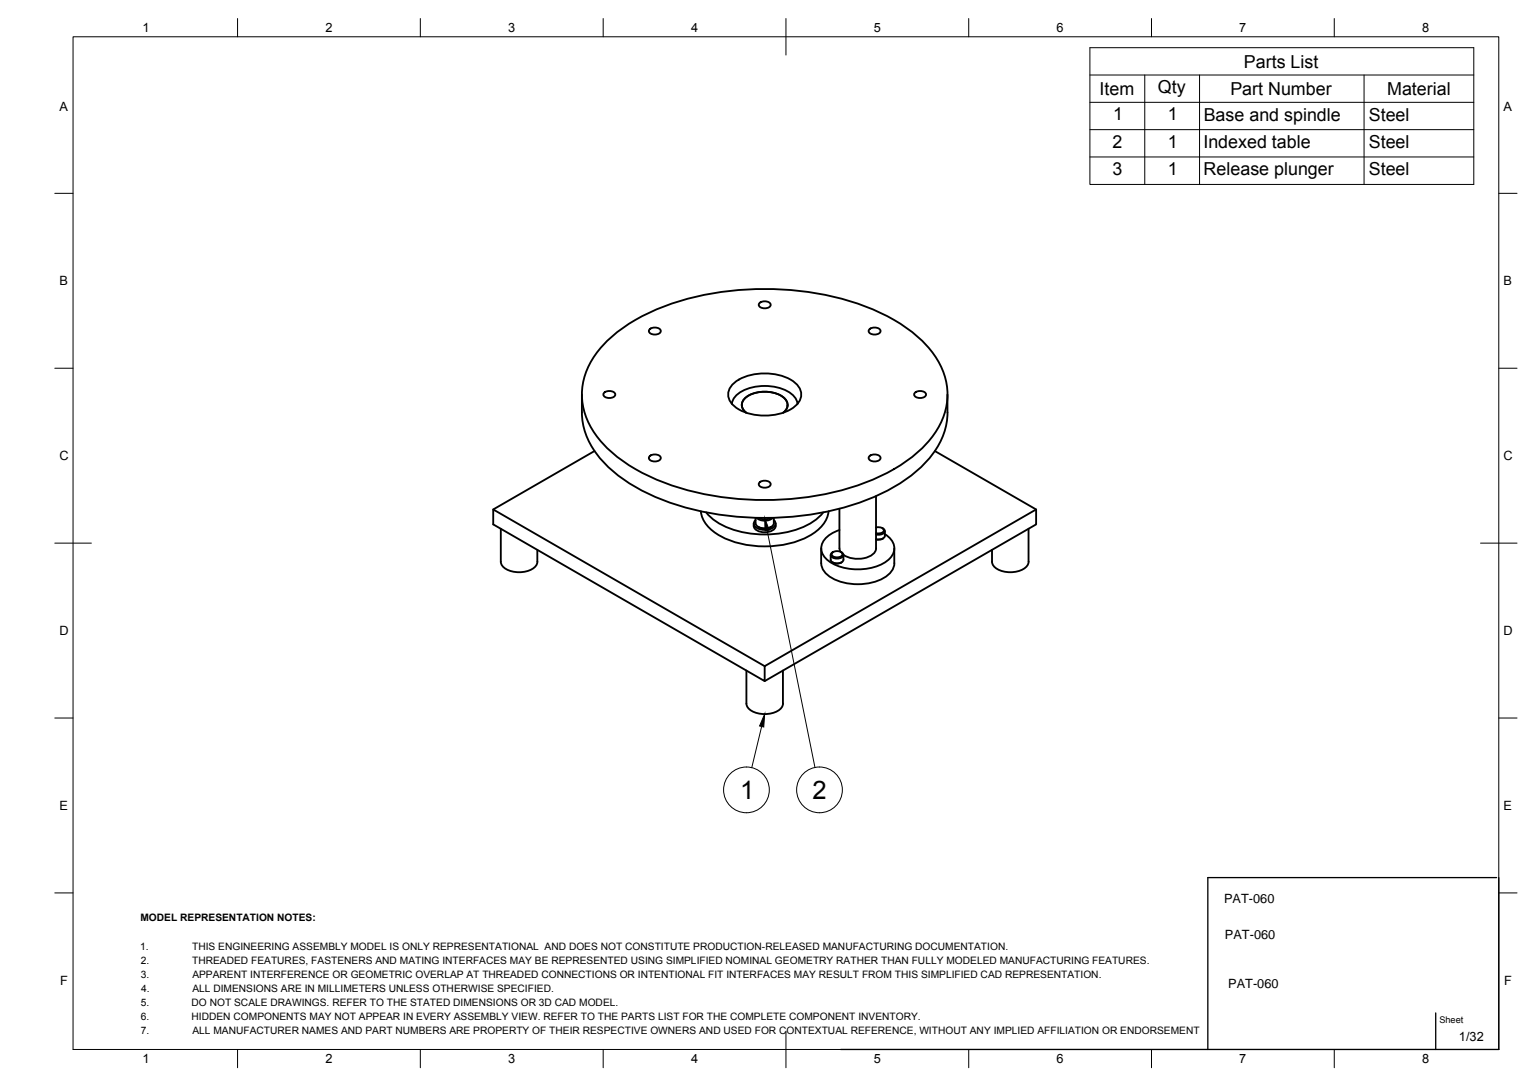
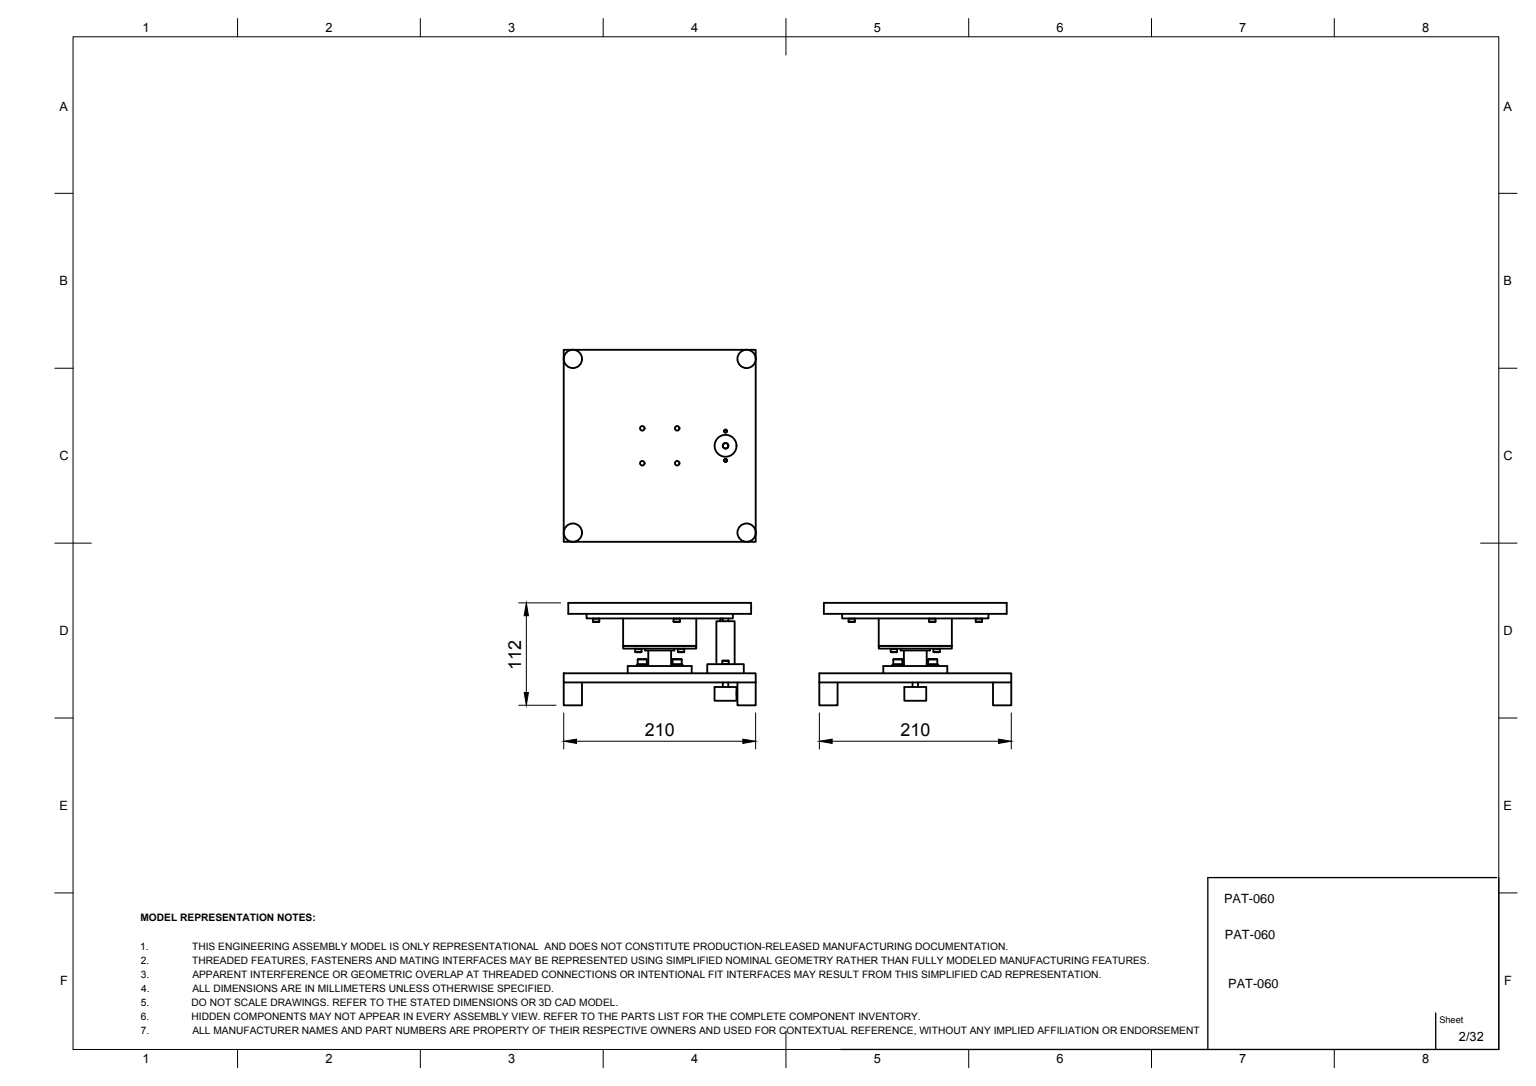
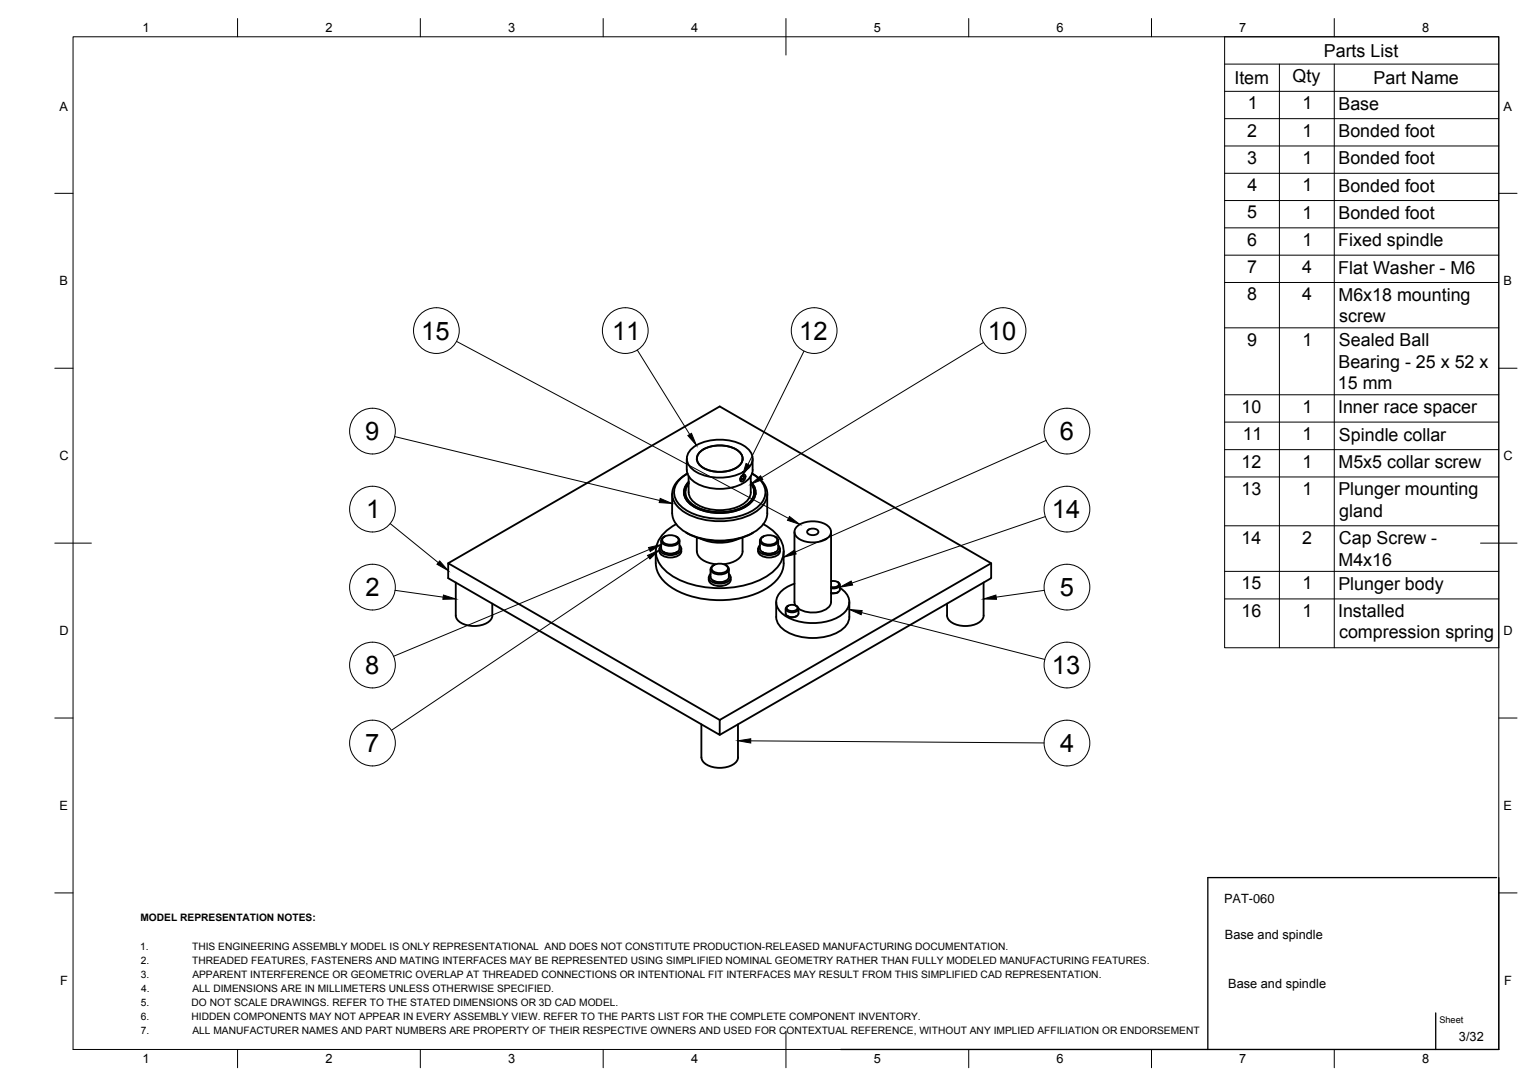
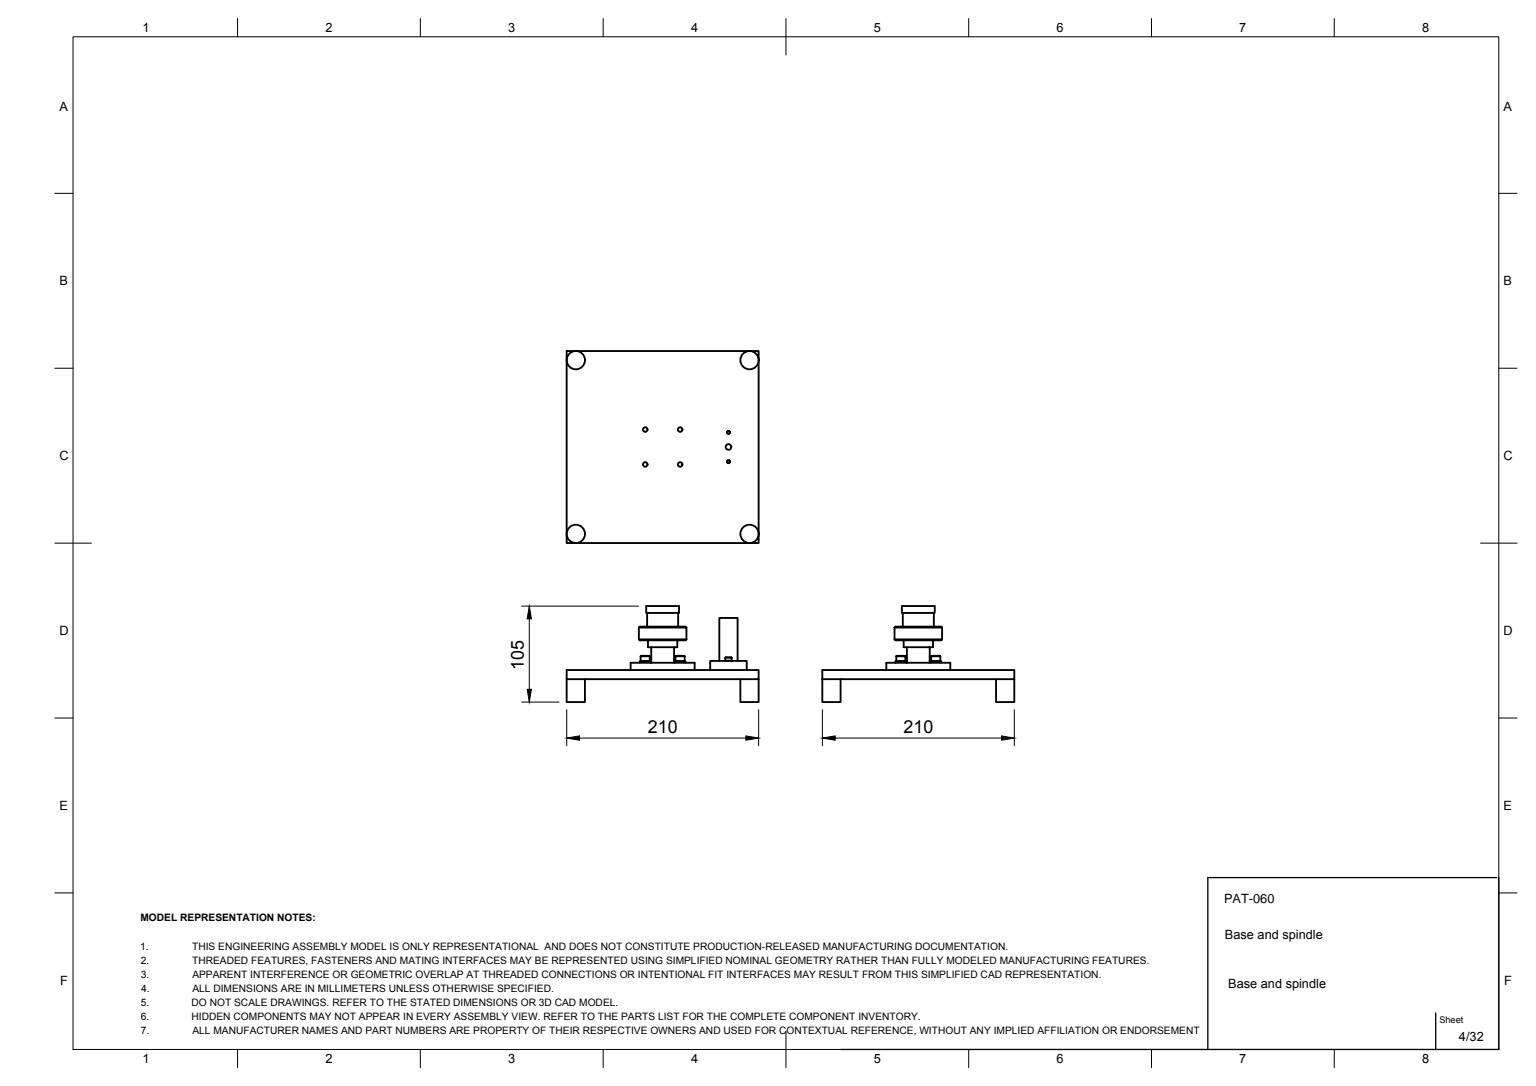
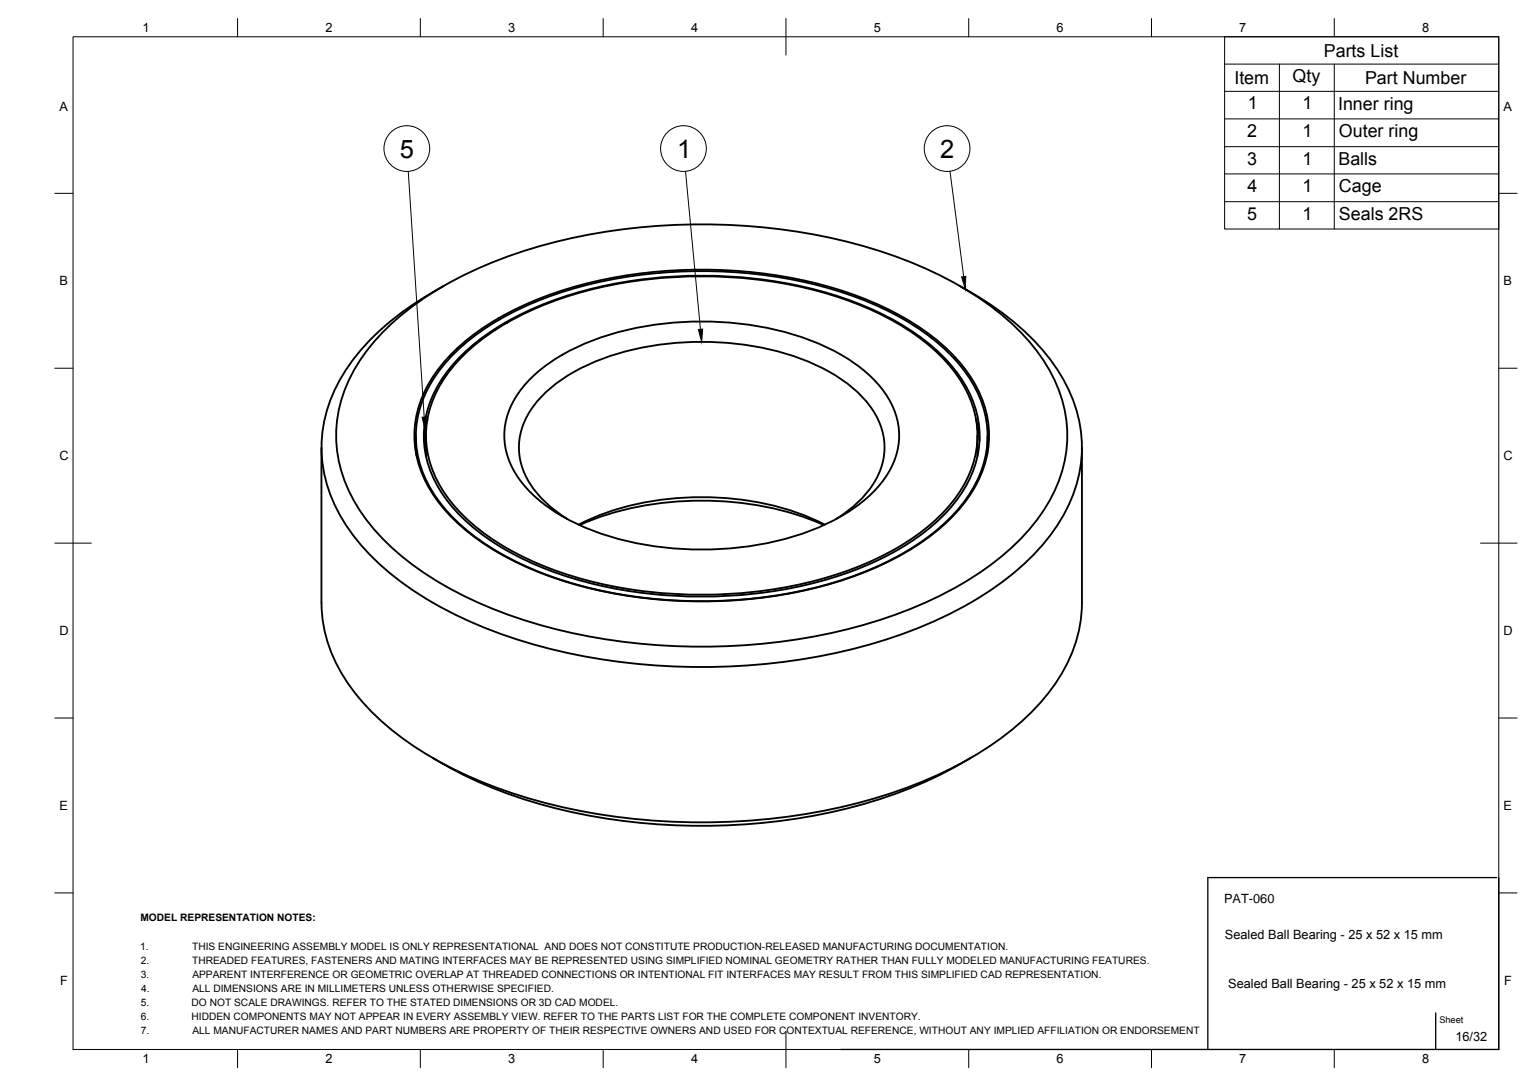
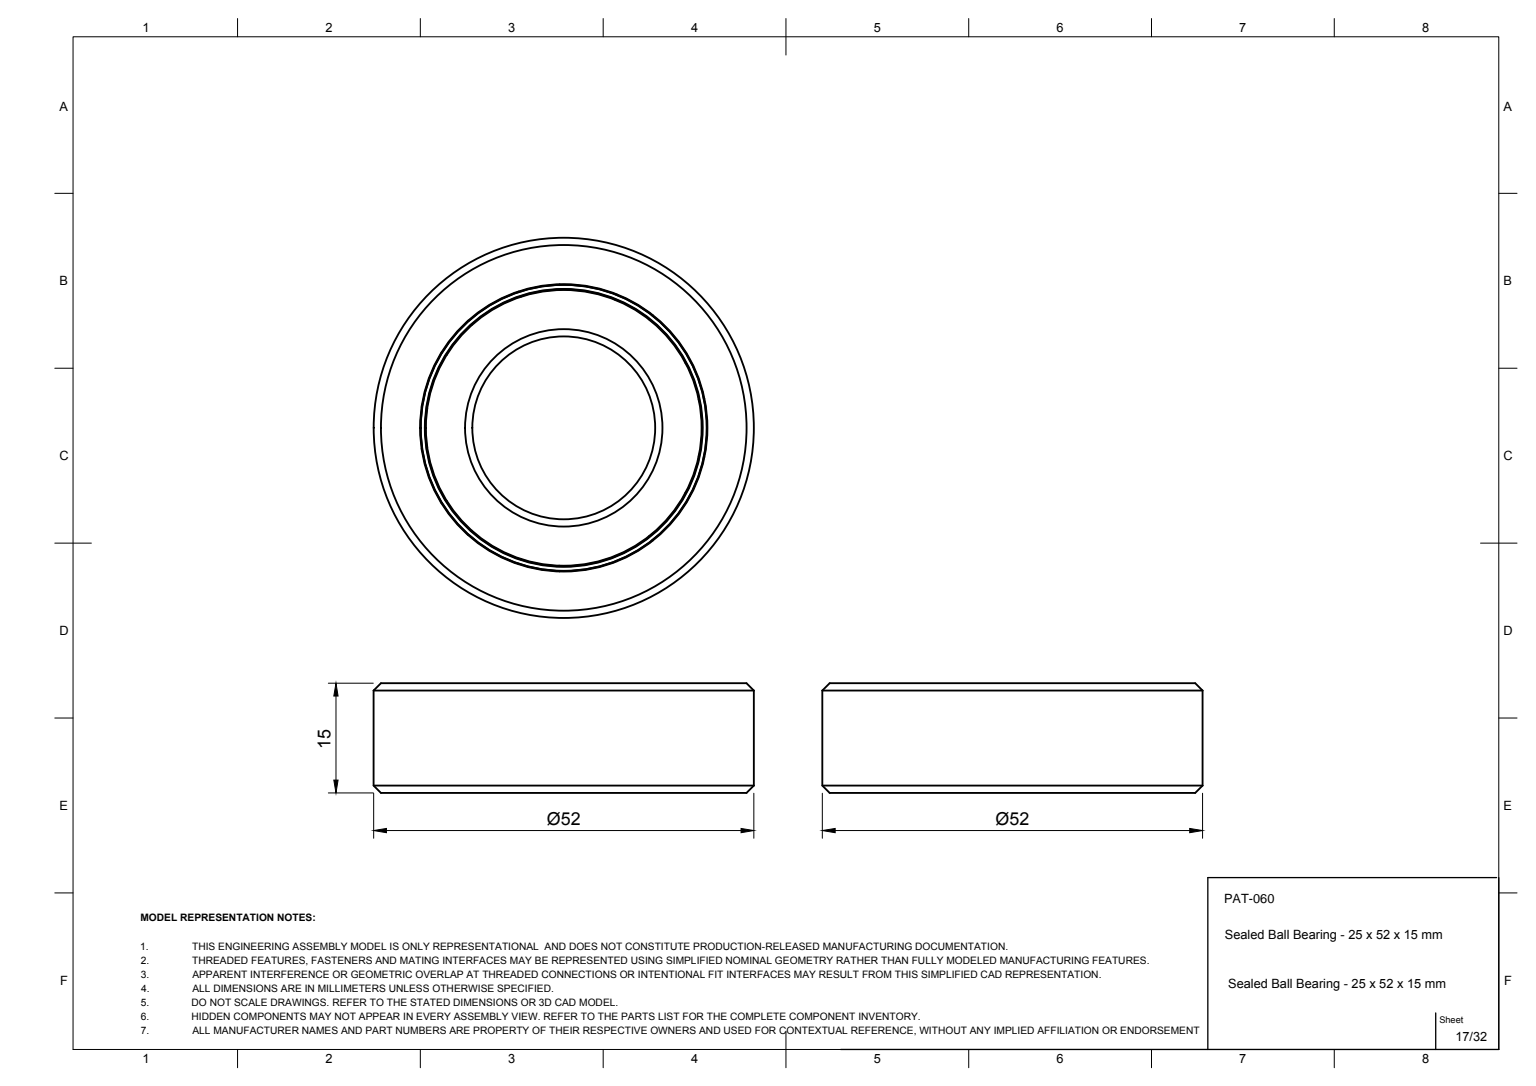
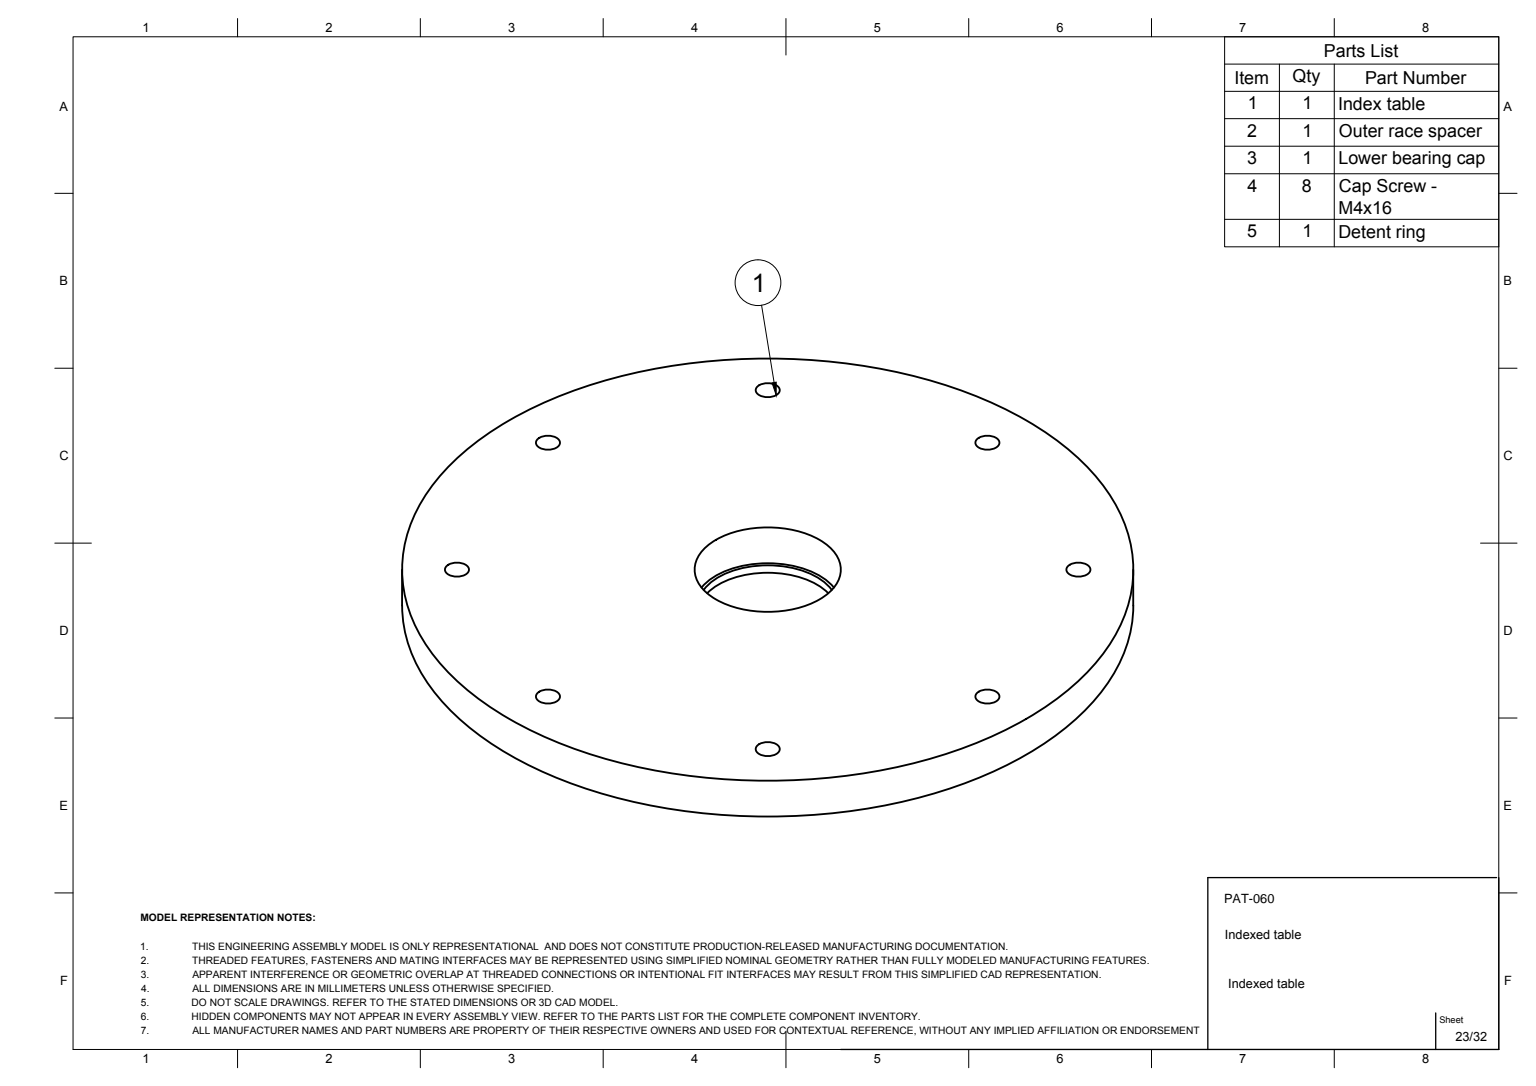
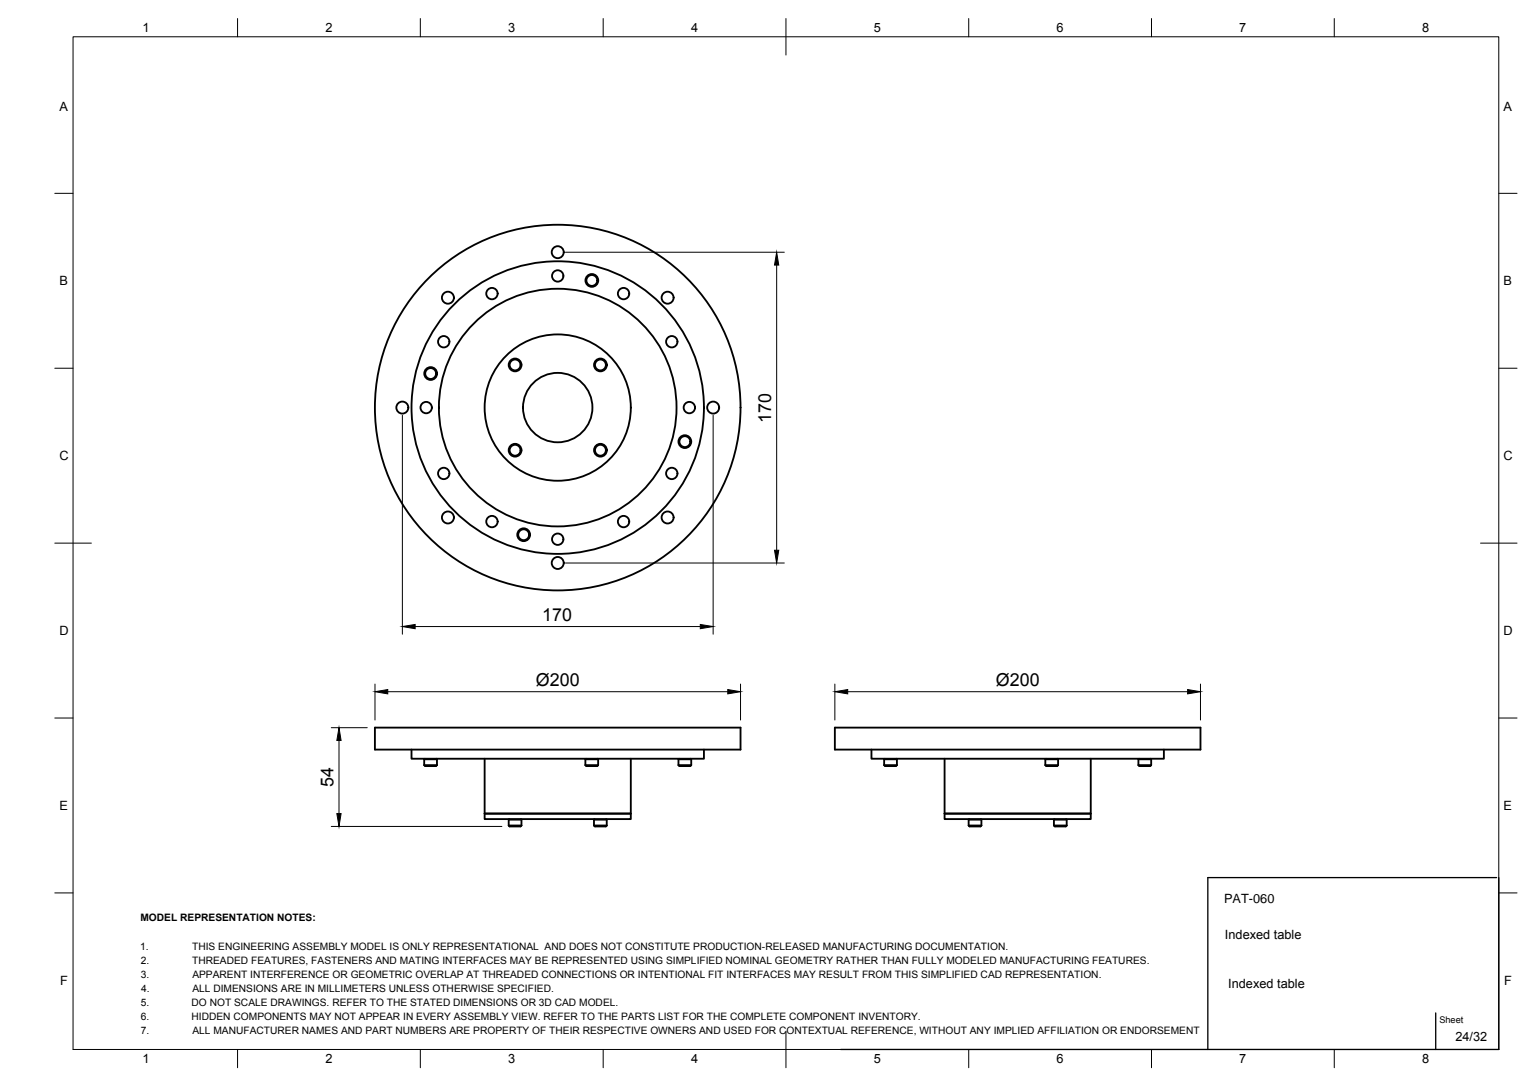
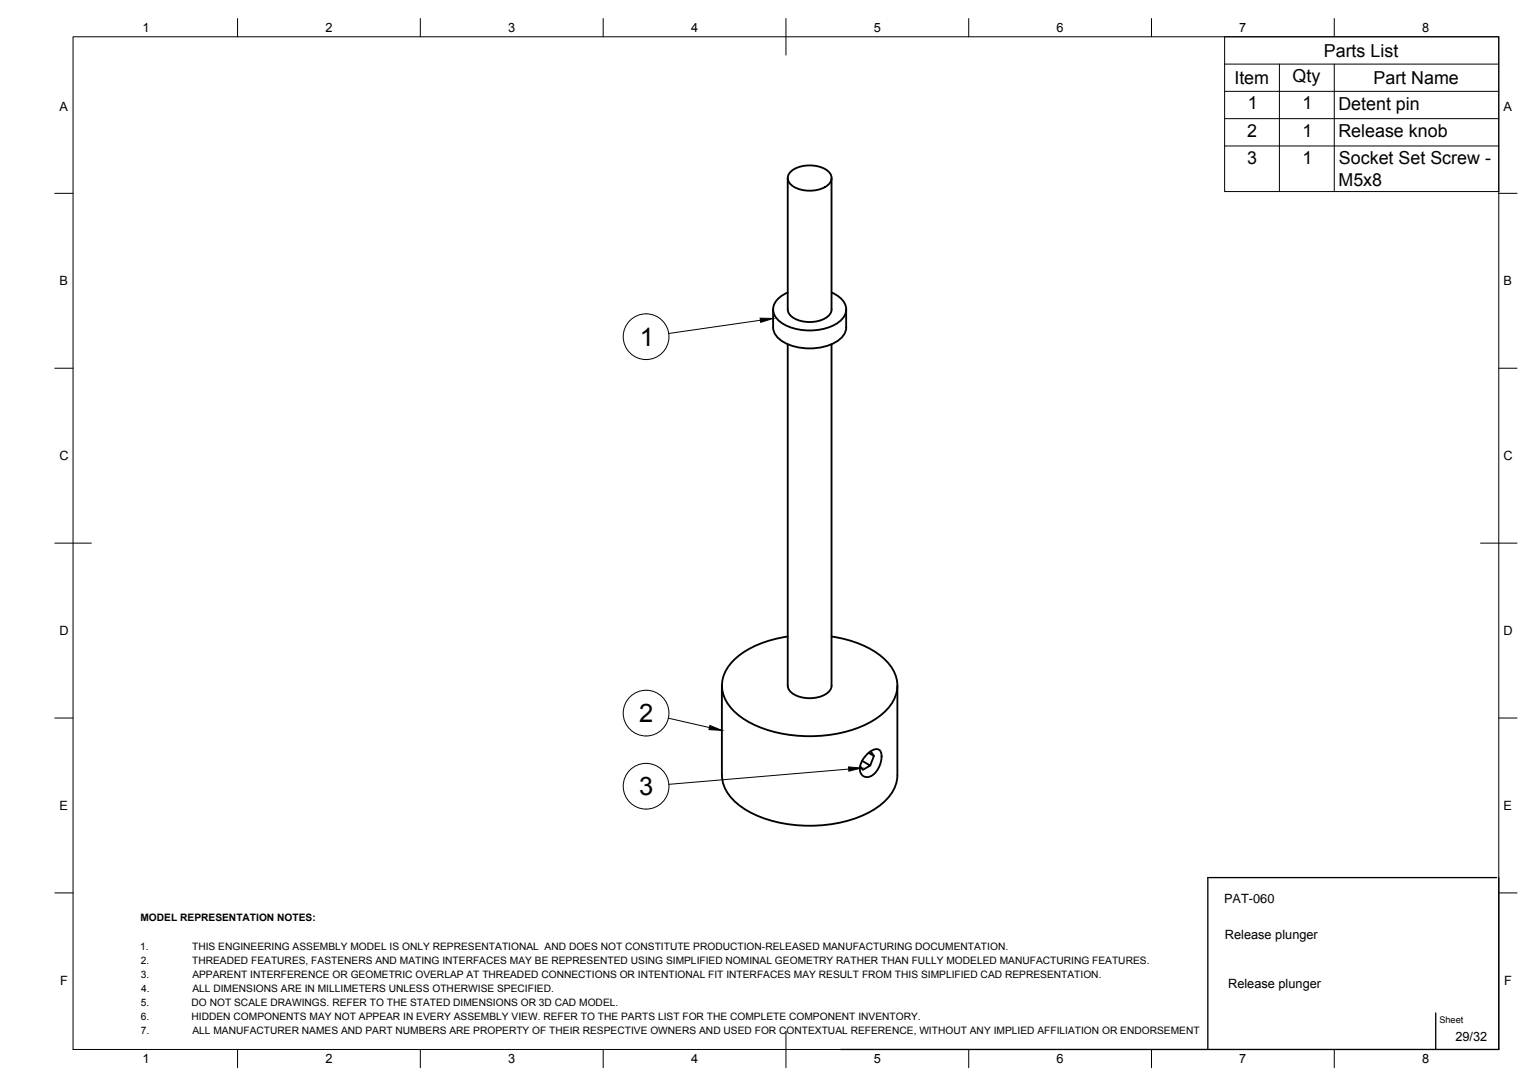
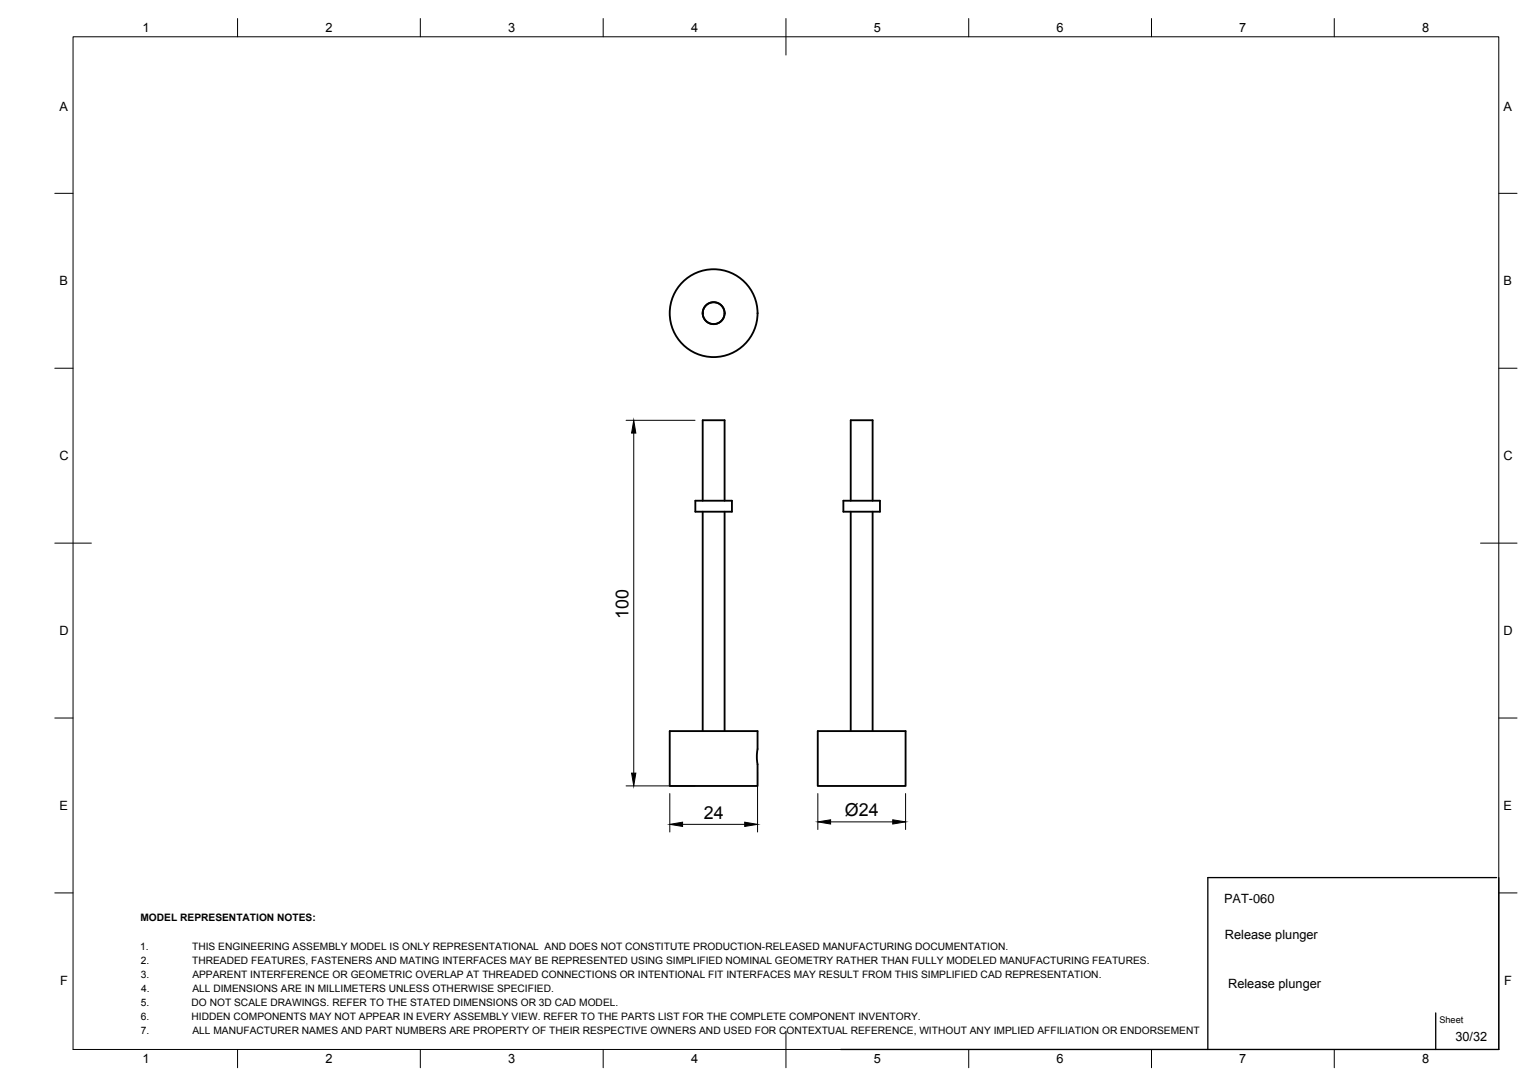
ISO-10303-21;
HEADER;
/* Generated by software containing ST-Developer
 * from STEP Tools, Inc. (www.steptools.com) 
 */

FILE_DESCRIPTION(
/* description */ ('Indexing fixture plate with plunger'),
/* implementation_level */ '2;1');

FILE_NAME(
/* name */ 'PAT-060',
/* time_stamp */ '2026-10-28T03:23:41-07:00',
/* author */ (''),
/* organization */ (''),
/* preprocessor_version */ 'ST-DEVELOPER v20.2',
/* originating_system */ 'Autodesk Translation Framework v15.17.0.0',
/* authorisation */ '');

FILE_SCHEMA (('AUTOMOTIVE_DESIGN { 1 0 10303 214 3 1 1 }'));
ENDSEC;

DATA;
#10=MECHANICAL_DESIGN_GEOMETRIC_PRESENTATION_REPRESENTATION('',(#317,#318,
#319,#320,#321,#322,#323,#324,#325,#326,#327,#328,#329,#330,#331,#332,#333,
#334,#335,#336,#337,#338,#339,#340,#341,#342,#343,#344,#345,#346,#347,#348,
#349,#350,#351,#352),#10020);
#11=ITEM_DEFINED_TRANSFORMATION($,$,#5085,#5223);
#12=ITEM_DEFINED_TRANSFORMATION($,$,#5105,#5224);
#13=ITEM_DEFINED_TRANSFORMATION($,$,#5125,#5225);
#14=ITEM_DEFINED_TRANSFORMATION($,$,#5144,#5226);
#15=ITEM_DEFINED_TRANSFORMATION($,$,#5206,#5227);
#16=ITEM_DEFINED_TRANSFORMATION($,$,#4909,#5486);
#17=ITEM_DEFINED_TRANSFORMATION($,$,#4937,#5487);
#18=ITEM_DEFINED_TRANSFORMATION($,$,#4943,#5488);
#19=ITEM_DEFINED_TRANSFORMATION($,$,#4949,#5489);
#20=ITEM_DEFINED_TRANSFORMATION($,$,#4955,#5490);
#21=ITEM_DEFINED_TRANSFORMATION($,$,#4961,#5491);
#22=ITEM_DEFINED_TRANSFORMATION($,$,#4991,#5492);
#23=ITEM_DEFINED_TRANSFORMATION($,$,#5000,#5493);
#24=ITEM_DEFINED_TRANSFORMATION($,$,#5014,#5494);
#25=ITEM_DEFINED_TRANSFORMATION($,$,#5033,#5495);
#26=ITEM_DEFINED_TRANSFORMATION($,$,#5046,#5496);
#27=ITEM_DEFINED_TRANSFORMATION($,$,#5051,#5497);
#28=ITEM_DEFINED_TRANSFORMATION($,$,#5060,#5498);
#29=ITEM_DEFINED_TRANSFORMATION($,$,#5051,#5499);
#30=ITEM_DEFINED_TRANSFORMATION($,$,#5060,#5500);
#31=ITEM_DEFINED_TRANSFORMATION($,$,#5051,#5501);
#32=ITEM_DEFINED_TRANSFORMATION($,$,#5060,#5502);
#33=ITEM_DEFINED_TRANSFORMATION($,$,#5051,#5503);
#34=ITEM_DEFINED_TRANSFORMATION($,$,#5060,#5504);
#35=ITEM_DEFINED_TRANSFORMATION($,$,#5084,#5505);
#36=ITEM_DEFINED_TRANSFORMATION($,$,#5228,#5506);
#37=ITEM_DEFINED_TRANSFORMATION($,$,#5460,#5507);
#38=ITEM_DEFINED_TRANSFORMATION($,$,#5460,#5508);
#39=ITEM_DEFINED_TRANSFORMATION($,$,#5244,#5509);
#40=ITEM_DEFINED_TRANSFORMATION($,$,#5369,#5510);
#41=ITEM_DEFINED_TRANSFORMATION($,$,#5378,#5511);
#42=ITEM_DEFINED_TRANSFORMATION($,$,#5403,#5512);
#43=ITEM_DEFINED_TRANSFORMATION($,$,#5460,#5513);
#44=ITEM_DEFINED_TRANSFORMATION($,$,#5460,#5514);
#45=ITEM_DEFINED_TRANSFORMATION($,$,#5460,#5515);
#46=ITEM_DEFINED_TRANSFORMATION($,$,#5460,#5516);
#47=ITEM_DEFINED_TRANSFORMATION($,$,#5460,#5517);
#48=ITEM_DEFINED_TRANSFORMATION($,$,#5460,#5518);
#49=ITEM_DEFINED_TRANSFORMATION($,$,#5460,#5519);
#50=ITEM_DEFINED_TRANSFORMATION($,$,#5460,#5520);
#51=ITEM_DEFINED_TRANSFORMATION($,$,#5522,#5567);
#52=ITEM_DEFINED_TRANSFORMATION($,$,#5536,#5568);
#53=ITEM_DEFINED_TRANSFORMATION($,$,#5550,#5569);
#54=ITEM_DEFINED_TRANSFORMATION($,$,#4908,#5570);
#55=ITEM_DEFINED_TRANSFORMATION($,$,#5243,#5571);
#56=ITEM_DEFINED_TRANSFORMATION($,$,#5521,#5572);
#57=(
REPRESENTATION_RELATIONSHIP($,$,#10151,#10150)
REPRESENTATION_RELATIONSHIP_WITH_TRANSFORMATION(#11)
SHAPE_REPRESENTATION_RELATIONSHIP()
);
#58=(
REPRESENTATION_RELATIONSHIP($,$,#10152,#10150)
REPRESENTATION_RELATIONSHIP_WITH_TRANSFORMATION(#12)
SHAPE_REPRESENTATION_RELATIONSHIP()
);
#59=(
REPRESENTATION_RELATIONSHIP($,$,#10153,#10150)
REPRESENTATION_RELATIONSHIP_WITH_TRANSFORMATION(#13)
SHAPE_REPRESENTATION_RELATIONSHIP()
);
#60=(
REPRESENTATION_RELATIONSHIP($,$,#10154,#10150)
REPRESENTATION_RELATIONSHIP_WITH_TRANSFORMATION(#14)
SHAPE_REPRESENTATION_RELATIONSHIP()
);
#61=(
REPRESENTATION_RELATIONSHIP($,$,#10155,#10150)
REPRESENTATION_RELATIONSHIP_WITH_TRANSFORMATION(#15)
SHAPE_REPRESENTATION_RELATIONSHIP()
);
#62=(
REPRESENTATION_RELATIONSHIP($,$,#10137,#10136)
REPRESENTATION_RELATIONSHIP_WITH_TRANSFORMATION(#16)
SHAPE_REPRESENTATION_RELATIONSHIP()
);
#63=(
REPRESENTATION_RELATIONSHIP($,$,#10138,#10136)
REPRESENTATION_RELATIONSHIP_WITH_TRANSFORMATION(#17)
SHAPE_REPRESENTATION_RELATIONSHIP()
);
#64=(
REPRESENTATION_RELATIONSHIP($,$,#10139,#10136)
REPRESENTATION_RELATIONSHIP_WITH_TRANSFORMATION(#18)
SHAPE_REPRESENTATION_RELATIONSHIP()
);
#65=(
REPRESENTATION_RELATIONSHIP($,$,#10140,#10136)
REPRESENTATION_RELATIONSHIP_WITH_TRANSFORMATION(#19)
SHAPE_REPRESENTATION_RELATIONSHIP()
);
#66=(
REPRESENTATION_RELATIONSHIP($,$,#10141,#10136)
REPRESENTATION_RELATIONSHIP_WITH_TRANSFORMATION(#20)
SHAPE_REPRESENTATION_RELATIONSHIP()
);
#67=(
REPRESENTATION_RELATIONSHIP($,$,#10142,#10136)
REPRESENTATION_RELATIONSHIP_WITH_TRANSFORMATION(#21)
SHAPE_REPRESENTATION_RELATIONSHIP()
);
#68=(
REPRESENTATION_RELATIONSHIP($,$,#10143,#10136)
REPRESENTATION_RELATIONSHIP_WITH_TRANSFORMATION(#22)
SHAPE_REPRESENTATION_RELATIONSHIP()
);
#69=(
REPRESENTATION_RELATIONSHIP($,$,#10144,#10136)
REPRESENTATION_RELATIONSHIP_WITH_TRANSFORMATION(#23)
SHAPE_REPRESENTATION_RELATIONSHIP()
);
#70=(
REPRESENTATION_RELATIONSHIP($,$,#10145,#10136)
REPRESENTATION_RELATIONSHIP_WITH_TRANSFORMATION(#24)
SHAPE_REPRESENTATION_RELATIONSHIP()
);
#71=(
REPRESENTATION_RELATIONSHIP($,$,#10146,#10136)
REPRESENTATION_RELATIONSHIP_WITH_TRANSFORMATION(#25)
SHAPE_REPRESENTATION_RELATIONSHIP()
);
#72=(
REPRESENTATION_RELATIONSHIP($,$,#10147,#10136)
REPRESENTATION_RELATIONSHIP_WITH_TRANSFORMATION(#26)
SHAPE_REPRESENTATION_RELATIONSHIP()
);
#73=(
REPRESENTATION_RELATIONSHIP($,$,#10148,#10136)
REPRESENTATION_RELATIONSHIP_WITH_TRANSFORMATION(#27)
SHAPE_REPRESENTATION_RELATIONSHIP()
);
#74=(
REPRESENTATION_RELATIONSHIP($,$,#10149,#10136)
REPRESENTATION_RELATIONSHIP_WITH_TRANSFORMATION(#28)
SHAPE_REPRESENTATION_RELATIONSHIP()
);
#75=(
REPRESENTATION_RELATIONSHIP($,$,#10148,#10136)
REPRESENTATION_RELATIONSHIP_WITH_TRANSFORMATION(#29)
SHAPE_REPRESENTATION_RELATIONSHIP()
);
#76=(
REPRESENTATION_RELATIONSHIP($,$,#10149,#10136)
REPRESENTATION_RELATIONSHIP_WITH_TRANSFORMATION(#30)
SHAPE_REPRESENTATION_RELATIONSHIP()
);
#77=(
REPRESENTATION_RELATIONSHIP($,$,#10148,#10136)
REPRESENTATION_RELATIONSHIP_WITH_TRANSFORMATION(#31)
SHAPE_REPRESENTATION_RELATIONSHIP()
);
#78=(
REPRESENTATION_RELATIONSHIP($,$,#10149,#10136)
REPRESENTATION_RELATIONSHIP_WITH_TRANSFORMATION(#32)
SHAPE_REPRESENTATION_RELATIONSHIP()
);
#79=(
REPRESENTATION_RELATIONSHIP($,$,#10148,#10136)
REPRESENTATION_RELATIONSHIP_WITH_TRANSFORMATION(#33)
SHAPE_REPRESENTATION_RELATIONSHIP()
);
#80=(
REPRESENTATION_RELATIONSHIP($,$,#10149,#10136)
REPRESENTATION_RELATIONSHIP_WITH_TRANSFORMATION(#34)
SHAPE_REPRESENTATION_RELATIONSHIP()
);
#81=(
REPRESENTATION_RELATIONSHIP($,$,#10150,#10136)
REPRESENTATION_RELATIONSHIP_WITH_TRANSFORMATION(#35)
SHAPE_REPRESENTATION_RELATIONSHIP()
);
#82=(
REPRESENTATION_RELATIONSHIP($,$,#10156,#10136)
REPRESENTATION_RELATIONSHIP_WITH_TRANSFORMATION(#36)
SHAPE_REPRESENTATION_RELATIONSHIP()
);
#83=(
REPRESENTATION_RELATIONSHIP($,$,#10162,#10136)
REPRESENTATION_RELATIONSHIP_WITH_TRANSFORMATION(#37)
SHAPE_REPRESENTATION_RELATIONSHIP()
);
#84=(
REPRESENTATION_RELATIONSHIP($,$,#10162,#10136)
REPRESENTATION_RELATIONSHIP_WITH_TRANSFORMATION(#38)
SHAPE_REPRESENTATION_RELATIONSHIP()
);
#85=(
REPRESENTATION_RELATIONSHIP($,$,#10158,#10157)
REPRESENTATION_RELATIONSHIP_WITH_TRANSFORMATION(#39)
SHAPE_REPRESENTATION_RELATIONSHIP()
);
#86=(
REPRESENTATION_RELATIONSHIP($,$,#10159,#10157)
REPRESENTATION_RELATIONSHIP_WITH_TRANSFORMATION(#40)
SHAPE_REPRESENTATION_RELATIONSHIP()
);
#87=(
REPRESENTATION_RELATIONSHIP($,$,#10160,#10157)
REPRESENTATION_RELATIONSHIP_WITH_TRANSFORMATION(#41)
SHAPE_REPRESENTATION_RELATIONSHIP()
);
#88=(
REPRESENTATION_RELATIONSHIP($,$,#10161,#10157)
REPRESENTATION_RELATIONSHIP_WITH_TRANSFORMATION(#42)
SHAPE_REPRESENTATION_RELATIONSHIP()
);
#89=(
REPRESENTATION_RELATIONSHIP($,$,#10162,#10157)
REPRESENTATION_RELATIONSHIP_WITH_TRANSFORMATION(#43)
SHAPE_REPRESENTATION_RELATIONSHIP()
);
#90=(
REPRESENTATION_RELATIONSHIP($,$,#10162,#10157)
REPRESENTATION_RELATIONSHIP_WITH_TRANSFORMATION(#44)
SHAPE_REPRESENTATION_RELATIONSHIP()
);
#91=(
REPRESENTATION_RELATIONSHIP($,$,#10162,#10157)
REPRESENTATION_RELATIONSHIP_WITH_TRANSFORMATION(#45)
SHAPE_REPRESENTATION_RELATIONSHIP()
);
#92=(
REPRESENTATION_RELATIONSHIP($,$,#10162,#10157)
REPRESENTATION_RELATIONSHIP_WITH_TRANSFORMATION(#46)
SHAPE_REPRESENTATION_RELATIONSHIP()
);
#93=(
REPRESENTATION_RELATIONSHIP($,$,#10162,#10157)
REPRESENTATION_RELATIONSHIP_WITH_TRANSFORMATION(#47)
SHAPE_REPRESENTATION_RELATIONSHIP()
);
#94=(
REPRESENTATION_RELATIONSHIP($,$,#10162,#10157)
REPRESENTATION_RELATIONSHIP_WITH_TRANSFORMATION(#48)
SHAPE_REPRESENTATION_RELATIONSHIP()
);
#95=(
REPRESENTATION_RELATIONSHIP($,$,#10162,#10157)
REPRESENTATION_RELATIONSHIP_WITH_TRANSFORMATION(#49)
SHAPE_REPRESENTATION_RELATIONSHIP()
);
#96=(
REPRESENTATION_RELATIONSHIP($,$,#10162,#10157)
REPRESENTATION_RELATIONSHIP_WITH_TRANSFORMATION(#50)
SHAPE_REPRESENTATION_RELATIONSHIP()
);
#97=(
REPRESENTATION_RELATIONSHIP($,$,#10164,#10163)
REPRESENTATION_RELATIONSHIP_WITH_TRANSFORMATION(#51)
SHAPE_REPRESENTATION_RELATIONSHIP()
);
#98=(
REPRESENTATION_RELATIONSHIP($,$,#10165,#10163)
REPRESENTATION_RELATIONSHIP_WITH_TRANSFORMATION(#52)
SHAPE_REPRESENTATION_RELATIONSHIP()
);
#99=(
REPRESENTATION_RELATIONSHIP($,$,#10166,#10163)
REPRESENTATION_RELATIONSHIP_WITH_TRANSFORMATION(#53)
SHAPE_REPRESENTATION_RELATIONSHIP()
);
#100=(
REPRESENTATION_RELATIONSHIP($,$,#10136,#10135)
REPRESENTATION_RELATIONSHIP_WITH_TRANSFORMATION(#54)
SHAPE_REPRESENTATION_RELATIONSHIP()
);
#101=(
REPRESENTATION_RELATIONSHIP($,$,#10157,#10135)
REPRESENTATION_RELATIONSHIP_WITH_TRANSFORMATION(#55)
SHAPE_REPRESENTATION_RELATIONSHIP()
);
#102=(
REPRESENTATION_RELATIONSHIP($,$,#10163,#10135)
REPRESENTATION_RELATIONSHIP_WITH_TRANSFORMATION(#56)
SHAPE_REPRESENTATION_RELATIONSHIP()
);
#103=CONTEXT_DEPENDENT_SHAPE_REPRESENTATION(#57,#10078);
#104=CONTEXT_DEPENDENT_SHAPE_REPRESENTATION(#58,#10079);
#105=CONTEXT_DEPENDENT_SHAPE_REPRESENTATION(#59,#10080);
#106=CONTEXT_DEPENDENT_SHAPE_REPRESENTATION(#60,#10081);
#107=CONTEXT_DEPENDENT_SHAPE_REPRESENTATION(#61,#10082);
#108=CONTEXT_DEPENDENT_SHAPE_REPRESENTATION(#62,#10090);
#109=CONTEXT_DEPENDENT_SHAPE_REPRESENTATION(#63,#10091);
#110=CONTEXT_DEPENDENT_SHAPE_REPRESENTATION(#64,#10092);
#111=CONTEXT_DEPENDENT_SHAPE_REPRESENTATION(#65,#10093);
#112=CONTEXT_DEPENDENT_SHAPE_REPRESENTATION(#66,#10094);
#113=CONTEXT_DEPENDENT_SHAPE_REPRESENTATION(#67,#10095);
#114=CONTEXT_DEPENDENT_SHAPE_REPRESENTATION(#68,#10096);
#115=CONTEXT_DEPENDENT_SHAPE_REPRESENTATION(#69,#10097);
#116=CONTEXT_DEPENDENT_SHAPE_REPRESENTATION(#70,#10098);
#117=CONTEXT_DEPENDENT_SHAPE_REPRESENTATION(#71,#10099);
#118=CONTEXT_DEPENDENT_SHAPE_REPRESENTATION(#72,#10100);
#119=CONTEXT_DEPENDENT_SHAPE_REPRESENTATION(#73,#10101);
#120=CONTEXT_DEPENDENT_SHAPE_REPRESENTATION(#74,#10102);
#121=CONTEXT_DEPENDENT_SHAPE_REPRESENTATION(#75,#10103);
#122=CONTEXT_DEPENDENT_SHAPE_REPRESENTATION(#76,#10104);
#123=CONTEXT_DEPENDENT_SHAPE_REPRESENTATION(#77,#10105);
#124=CONTEXT_DEPENDENT_SHAPE_REPRESENTATION(#78,#10106);
#125=CONTEXT_DEPENDENT_SHAPE_REPRESENTATION(#79,#10107);
#126=CONTEXT_DEPENDENT_SHAPE_REPRESENTATION(#80,#10108);
#127=CONTEXT_DEPENDENT_SHAPE_REPRESENTATION(#81,#10109);
#128=CONTEXT_DEPENDENT_SHAPE_REPRESENTATION(#82,#10110);
#129=CONTEXT_DEPENDENT_SHAPE_REPRESENTATION(#83,#10111);
#130=CONTEXT_DEPENDENT_SHAPE_REPRESENTATION(#84,#10112);
#131=CONTEXT_DEPENDENT_SHAPE_REPRESENTATION(#85,#10113);
#132=CONTEXT_DEPENDENT_SHAPE_REPRESENTATION(#86,#10114);
#133=CONTEXT_DEPENDENT_SHAPE_REPRESENTATION(#87,#10115);
#134=CONTEXT_DEPENDENT_SHAPE_REPRESENTATION(#88,#10116);
#135=CONTEXT_DEPENDENT_SHAPE_REPRESENTATION(#89,#10117);
#136=CONTEXT_DEPENDENT_SHAPE_REPRESENTATION(#90,#10118);
#137=CONTEXT_DEPENDENT_SHAPE_REPRESENTATION(#91,#10119);
#138=CONTEXT_DEPENDENT_SHAPE_REPRESENTATION(#92,#10120);
#139=CONTEXT_DEPENDENT_SHAPE_REPRESENTATION(#93,#10121);
#140=CONTEXT_DEPENDENT_SHAPE_REPRESENTATION(#94,#10122);
#141=CONTEXT_DEPENDENT_SHAPE_REPRESENTATION(#95,#10123);
#142=CONTEXT_DEPENDENT_SHAPE_REPRESENTATION(#96,#10124);
#143=CONTEXT_DEPENDENT_SHAPE_REPRESENTATION(#97,#10129);
#144=CONTEXT_DEPENDENT_SHAPE_REPRESENTATION(#98,#10130);
#145=CONTEXT_DEPENDENT_SHAPE_REPRESENTATION(#99,#10131);
#146=CONTEXT_DEPENDENT_SHAPE_REPRESENTATION(#100,#10132);
#147=CONTEXT_DEPENDENT_SHAPE_REPRESENTATION(#101,#10133);
#148=CONTEXT_DEPENDENT_SHAPE_REPRESENTATION(#102,#10134);
#149=NEXT_ASSEMBLY_USAGE_OCCURRENCE('Inner ring:1','Inner ring:1',
'Inner ring:1',#10183,#10184,'Inner ring:1');
#150=NEXT_ASSEMBLY_USAGE_OCCURRENCE('Outer ring:1','Outer ring:1',
'Outer ring:1',#10183,#10185,'Outer ring:1');
#151=NEXT_ASSEMBLY_USAGE_OCCURRENCE('Balls:1','Balls:1','Balls:1',#10183,
#10186,'Balls:1');
#152=NEXT_ASSEMBLY_USAGE_OCCURRENCE('Cage:1','Cage:1','Cage:1',#10183,#10187,
'Cage:1');
#153=NEXT_ASSEMBLY_USAGE_OCCURRENCE('Seals 2RS:1','Seals 2RS:1',
'Seals 2RS:1',#10183,#10188,'Seals 2RS:1');
#154=NEXT_ASSEMBLY_USAGE_OCCURRENCE('Base:1','Base:1','Base:1',#10169,#10170,
'Base:1');
#155=NEXT_ASSEMBLY_USAGE_OCCURRENCE('Bonded foot:1','Bonded foot:1',
'Bonded foot:1',#10169,#10171,'Bonded foot:1');
#156=NEXT_ASSEMBLY_USAGE_OCCURRENCE('Bonded foot (1):1',
'Bonded foot (1):1','Bonded foot (1):1',#10169,#10172,
'Bonded foot (1):1');
#157=NEXT_ASSEMBLY_USAGE_OCCURRENCE('Bonded foot (2):1',
'Bonded foot (2):1','Bonded foot (2):1',#10169,#10173,
'Bonded foot (2):1');
#158=NEXT_ASSEMBLY_USAGE_OCCURRENCE('Bonded foot (3):1',
'Bonded foot (3):1','Bonded foot (3):1',#10169,#10174,
'Bonded foot (3):1');
#159=NEXT_ASSEMBLY_USAGE_OCCURRENCE('Fixed spindle:1','Fixed spindle:1',
'Fixed spindle:1',#10169,#10175,'Fixed spindle:1');
#160=NEXT_ASSEMBLY_USAGE_OCCURRENCE('Inner race spacer:1',
'Inner race spacer:1','Inner race spacer:1',#10169,#10176,
'Inner race spacer:1');
#161=NEXT_ASSEMBLY_USAGE_OCCURRENCE('Spindle collar:1',
'Spindle collar:1','Spindle collar:1',#10169,#10177,'Spindle collar:1');
#162=NEXT_ASSEMBLY_USAGE_OCCURRENCE('Plunger mounting gland:1',
'Plunger mounting gland:1','Plunger mounting gland:1',#10169,#10178,
'Plunger mounting gland:1');
#163=NEXT_ASSEMBLY_USAGE_OCCURRENCE('Plunger body:1','Plunger body:1',
'Plunger body:1',#10169,#10179,'Plunger body:1');
#164=NEXT_ASSEMBLY_USAGE_OCCURRENCE('Installed compression spring:1',
'Installed compression spring:1','Installed compression spring:1',#10169,
#10180,'Installed compression spring:1');
#165=NEXT_ASSEMBLY_USAGE_OCCURRENCE('Flat Washer - M6:2',
'Flat Washer - M6:2','Flat Washer - M6:2',#10169,#10181,
'Flat Washer - M6:2');
#166=NEXT_ASSEMBLY_USAGE_OCCURRENCE('M6x18 mounting screw:2',
'M6x18 mounting screw:2','M6x18 mounting screw:2',#10169,#10182,
'M6x18 mounting screw:2');
#167=NEXT_ASSEMBLY_USAGE_OCCURRENCE('Flat Washer - M6:3',
'Flat Washer - M6:3','Flat Washer - M6:3',#10169,#10181,
'Flat Washer - M6:3');
#168=NEXT_ASSEMBLY_USAGE_OCCURRENCE('M6x18 mounting screw:3',
'M6x18 mounting screw:3','M6x18 mounting screw:3',#10169,#10182,
'M6x18 mounting screw:3');
#169=NEXT_ASSEMBLY_USAGE_OCCURRENCE('Flat Washer - M6:4',
'Flat Washer - M6:4','Flat Washer - M6:4',#10169,#10181,
'Flat Washer - M6:4');
#170=NEXT_ASSEMBLY_USAGE_OCCURRENCE('M6x18 mounting screw:4',
'M6x18 mounting screw:4','M6x18 mounting screw:4',#10169,#10182,
'M6x18 mounting screw:4');
#171=NEXT_ASSEMBLY_USAGE_OCCURRENCE('Flat Washer - M6:5',
'Flat Washer - M6:5','Flat Washer - M6:5',#10169,#10181,
'Flat Washer - M6:5');
#172=NEXT_ASSEMBLY_USAGE_OCCURRENCE('M6x18 mounting screw:5',
'M6x18 mounting screw:5','M6x18 mounting screw:5',#10169,#10182,
'M6x18 mounting screw:5');
#173=NEXT_ASSEMBLY_USAGE_OCCURRENCE(
'Sealed Ball Bearing - 25 x 52 x 15 mm:2',
'Sealed Ball Bearing - 25 x 52 x 15 mm:2',
'Sealed Ball Bearing - 25 x 52 x 15 mm:2',#10169,#10183,
'Sealed Ball Bearing - 25 x 52 x 15 mm:2');
#174=NEXT_ASSEMBLY_USAGE_OCCURRENCE('M5x5 collar screw:2',
'M5x5 collar screw:2','M5x5 collar screw:2',#10169,#10189,
'M5x5 collar screw:2');
#175=NEXT_ASSEMBLY_USAGE_OCCURRENCE('Cap Screw - M4x16:10',
'Cap Screw - M4x16:10','Cap Screw - M4x16:10',#10169,#10195,
'Cap Screw - M4x16:10');
#176=NEXT_ASSEMBLY_USAGE_OCCURRENCE('Cap Screw - M4x16:11',
'Cap Screw - M4x16:11','Cap Screw - M4x16:11',#10169,#10195,
'Cap Screw - M4x16:11');
#177=NEXT_ASSEMBLY_USAGE_OCCURRENCE('Index table:1','Index table:1',
'Index table:1',#10190,#10191,'Index table:1');
#178=NEXT_ASSEMBLY_USAGE_OCCURRENCE('Outer race spacer:1',
'Outer race spacer:1','Outer race spacer:1',#10190,#10192,
'Outer race spacer:1');
#179=NEXT_ASSEMBLY_USAGE_OCCURRENCE('Lower bearing cap:1',
'Lower bearing cap:1','Lower bearing cap:1',#10190,#10193,
'Lower bearing cap:1');
#180=NEXT_ASSEMBLY_USAGE_OCCURRENCE('Detent ring:1','Detent ring:1',
'Detent ring:1',#10190,#10194,'Detent ring:1');
#181=NEXT_ASSEMBLY_USAGE_OCCURRENCE('Cap Screw - M4x16:2',
'Cap Screw - M4x16:2','Cap Screw - M4x16:2',#10190,#10195,
'Cap Screw - M4x16:2');
#182=NEXT_ASSEMBLY_USAGE_OCCURRENCE('Cap Screw - M4x16:3',
'Cap Screw - M4x16:3','Cap Screw - M4x16:3',#10190,#10195,
'Cap Screw - M4x16:3');
#183=NEXT_ASSEMBLY_USAGE_OCCURRENCE('Cap Screw - M4x16:4',
'Cap Screw - M4x16:4','Cap Screw - M4x16:4',#10190,#10195,
'Cap Screw - M4x16:4');
#184=NEXT_ASSEMBLY_USAGE_OCCURRENCE('Cap Screw - M4x16:5',
'Cap Screw - M4x16:5','Cap Screw - M4x16:5',#10190,#10195,
'Cap Screw - M4x16:5');
#185=NEXT_ASSEMBLY_USAGE_OCCURRENCE('Cap Screw - M4x16:6',
'Cap Screw - M4x16:6','Cap Screw - M4x16:6',#10190,#10195,
'Cap Screw - M4x16:6');
#186=NEXT_ASSEMBLY_USAGE_OCCURRENCE('Cap Screw - M4x16:7',
'Cap Screw - M4x16:7','Cap Screw - M4x16:7',#10190,#10195,
'Cap Screw - M4x16:7');
#187=NEXT_ASSEMBLY_USAGE_OCCURRENCE('Cap Screw - M4x16:8',
'Cap Screw - M4x16:8','Cap Screw - M4x16:8',#10190,#10195,
'Cap Screw - M4x16:8');
#188=NEXT_ASSEMBLY_USAGE_OCCURRENCE('Cap Screw - M4x16:9',
'Cap Screw - M4x16:9','Cap Screw - M4x16:9',#10190,#10195,
'Cap Screw - M4x16:9');
#189=NEXT_ASSEMBLY_USAGE_OCCURRENCE('Detent pin:1','Detent pin:1',
'Detent pin:1',#10196,#10197,'Detent pin:1');
#190=NEXT_ASSEMBLY_USAGE_OCCURRENCE('Release knob:1','Release knob:1',
'Release knob:1',#10196,#10198,'Release knob:1');
#191=NEXT_ASSEMBLY_USAGE_OCCURRENCE('Socket Set Screw - M5x8:2',
'Socket Set Screw - M5x8:2','Socket Set Screw - M5x8:2',#10196,#10199,
'Socket Set Screw - M5x8:2');
#192=NEXT_ASSEMBLY_USAGE_OCCURRENCE('Base and spindle:1',
'Base and spindle:1','Base and spindle:1',#10168,#10169,
'Base and spindle:1');
#193=NEXT_ASSEMBLY_USAGE_OCCURRENCE('Indexed table:1','Indexed table:1',
'Indexed table:1',#10168,#10190,'Indexed table:1');
#194=NEXT_ASSEMBLY_USAGE_OCCURRENCE('Release plunger:1',
'Release plunger:1','Release plunger:1',#10168,#10196,
'Release plunger:1');
#195=SPHERICAL_SURFACE('',#5126,0.3969);
#196=SPHERICAL_SURFACE('',#5128,0.3969);
#197=SPHERICAL_SURFACE('',#5130,0.3969);
#198=SPHERICAL_SURFACE('',#5132,0.3969);
#199=SPHERICAL_SURFACE('',#5134,0.3969);
#200=SPHERICAL_SURFACE('',#5136,0.3969);
#201=SPHERICAL_SURFACE('',#5138,0.3969);
#202=SPHERICAL_SURFACE('',#5140,0.3969);
#203=SPHERICAL_SURFACE('',#5142,0.3969);
#204=SPHERICAL_SURFACE('',#5145,0.412776);
#205=SPHERICAL_SURFACE('',#5163,0.412776);
#206=SPHERICAL_SURFACE('',#5168,0.412776);
#207=SPHERICAL_SURFACE('',#5173,0.412776);
#208=SPHERICAL_SURFACE('',#5179,0.412776);
#209=SPHERICAL_SURFACE('',#5184,0.412776);
#210=SPHERICAL_SURFACE('',#5189,0.412776);
#211=SPHERICAL_SURFACE('',#5194,0.412776);
#212=SPHERICAL_SURFACE('',#5202,0.412776);
#213=TOROIDAL_SURFACE('',#5086,1.925,0.412776);
#214=TOROIDAL_SURFACE('',#5106,1.925,0.412776);
#215=CONICAL_SURFACE('',#5073,0.475,0.785398163397449);
#216=CONICAL_SURFACE('',#5077,0.485,0.785398163397448);
#217=CONICAL_SURFACE('',#5081,0.31,0.463647609000806);
#218=CONICAL_SURFACE('',#5097,1.3,0.785398163397449);
#219=CONICAL_SURFACE('',#5104,1.3,0.785398163397449);
#220=CONICAL_SURFACE('',#5117,2.55,0.785398163397449);
#221=CONICAL_SURFACE('',#5121,2.55,0.785398163397449);
#222=CONICAL_SURFACE('',#5240,0.235,0.785398163397448);
#223=CONICAL_SURFACE('',#5463,0.325,0.785398163397448);
#224=CONICAL_SURFACE('',#5467,0.335,0.785398163397448);
#225=CONICAL_SURFACE('',#5471,0.21,0.463647609000806);
#226=CONICAL_SURFACE('',#5475,0.18,0.785398163397448);
#227=CONICAL_SURFACE('',#5560,0.235,0.785398163397448);
#228=CONICAL_SURFACE('',#5564,0.2125,0.785398163397448);
#229=ORIENTED_CLOSED_SHELL('',*,#4583,.F.);
#230=ORIENTED_CLOSED_SHELL('',*,#4605,.F.);
#231=BREP_WITH_VOIDS('Body1',#4584,(#229));
#232=BREP_WITH_VOIDS('Body1',#4604,(#230));
#233=B_SPLINE_SURFACE_WITH_KNOTS('',3,3,((#7454,#7455,#7456,#7457,#7458,
#7459,#7460,#7461,#7462,#7463,#7464,#7465,#7466,#7467,#7468,#7469,#7470,
#7471,#7472,#7473,#7474,#7475,#7476,#7477,#7478,#7479,#7480,#7481,#7482,
#7483,#7484,#7485,#7486,#7487,#7488,#7489,#7490,#7491,#7492,#7493,#7494,
#7495,#7496,#7497,#7498,#7499,#7500,#7501,#7502,#7503,#7504,#7505,#7506,
#7507,#7508,#7509,#7510,#7511,#7512,#7513,#7514,#7515,#7516,#7517,#7518,
#7519,#7520,#7521,#7522,#7523,#7524,#7525,#7526,#7527,#7528,#7529,#7530,
#7531,#7532,#7533,#7534,#7535,#7536,#7537,#7538,#7539,#7540,#7541,#7542,
#7543,#7544,#7545,#7546,#7547,#7548,#7549),(#7550,#7551,#7552,#7553,#7554,
#7555,#7556,#7557,#7558,#7559,#7560,#7561,#7562,#7563,#7564,#7565,#7566,
#7567,#7568,#7569,#7570,#7571,#7572,#7573,#7574,#7575,#7576,#7577,#7578,
#7579,#7580,#7581,#7582,#7583,#7584,#7585,#7586,#7587,#7588,#7589,#7590,
#7591,#7592,#7593,#7594,#7595,#7596,#7597,#7598,#7599,#7600,#7601,#7602,
#7603,#7604,#7605,#7606,#7607,#7608,#7609,#7610,#7611,#7612,#7613,#7614,
#7615,#7616,#7617,#7618,#7619,#7620,#7621,#7622,#7623,#7624,#7625,#7626,
#7627,#7628,#7629,#7630,#7631,#7632,#7633,#7634,#7635,#7636,#7637,#7638,
#7639,#7640,#7641,#7642,#7643,#7644,#7645),(#7646,#7647,#7648,#7649,#7650,
#7651,#7652,#7653,#7654,#7655,#7656,#7657,#7658,#7659,#7660,#7661,#7662,
#7663,#7664,#7665,#7666,#7667,#7668,#7669,#7670,#7671,#7672,#7673,#7674,
#7675,#7676,#7677,#7678,#7679,#7680,#7681,#7682,#7683,#7684,#7685,#7686,
#7687,#7688,#7689,#7690,#7691,#7692,#7693,#7694,#7695,#7696,#7697,#7698,
#7699,#7700,#7701,#7702,#7703,#7704,#7705,#7706,#7707,#7708,#7709,#7710,
#7711,#7712,#7713,#7714,#7715,#7716,#7717,#7718,#7719,#7720,#7721,#7722,
#7723,#7724,#7725,#7726,#7727,#7728,#7729,#7730,#7731,#7732,#7733,#7734,
#7735,#7736,#7737,#7738,#7739,#7740,#7741),(#7742,#7743,#7744,#7745,#7746,
#7747,#7748,#7749,#7750,#7751,#7752,#7753,#7754,#7755,#7756,#7757,#7758,
#7759,#7760,#7761,#7762,#7763,#7764,#7765,#7766,#7767,#7768,#7769,#7770,
#7771,#7772,#7773,#7774,#7775,#7776,#7777,#7778,#7779,#7780,#7781,#7782,
#7783,#7784,#7785,#7786,#7787,#7788,#7789,#7790,#7791,#7792,#7793,#7794,
#7795,#7796,#7797,#7798,#7799,#7800,#7801,#7802,#7803,#7804,#7805,#7806,
#7807,#7808,#7809,#7810,#7811,#7812,#7813,#7814,#7815,#7816,#7817,#7818,
#7819,#7820,#7821,#7822,#7823,#7824,#7825,#7826,#7827,#7828,#7829,#7830,
#7831,#7832,#7833,#7834,#7835,#7836,#7837),(#7838,#7839,#7840,#7841,#7842,
#7843,#7844,#7845,#7846,#7847,#7848,#7849,#7850,#7851,#7852,#7853,#7854,
#7855,#7856,#7857,#7858,#7859,#7860,#7861,#7862,#7863,#7864,#7865,#7866,
#7867,#7868,#7869,#7870,#7871,#7872,#7873,#7874,#7875,#7876,#7877,#7878,
#7879,#7880,#7881,#7882,#7883,#7884,#7885,#7886,#7887,#7888,#7889,#7890,
#7891,#7892,#7893,#7894,#7895,#7896,#7897,#7898,#7899,#7900,#7901,#7902,
#7903,#7904,#7905,#7906,#7907,#7908,#7909,#7910,#7911,#7912,#7913,#7914,
#7915,#7916,#7917,#7918,#7919,#7920,#7921,#7922,#7923,#7924,#7925,#7926,
#7927,#7928,#7929,#7930,#7931,#7932,#7933),(#7934,#7935,#7936,#7937,#7938,
#7939,#7940,#7941,#7942,#7943,#7944,#7945,#7946,#7947,#7948,#7949,#7950,
#7951,#7952,#7953,#7954,#7955,#7956,#7957,#7958,#7959,#7960,#7961,#7962,
#7963,#7964,#7965,#7966,#7967,#7968,#7969,#7970,#7971,#7972,#7973,#7974,
#7975,#7976,#7977,#7978,#7979,#7980,#7981,#7982,#7983,#7984,#7985,#7986,
#7987,#7988,#7989,#7990,#7991,#7992,#7993,#7994,#7995,#7996,#7997,#7998,
#7999,#8000,#8001,#8002,#8003,#8004,#8005,#8006,#8007,#8008,#8009,#8010,
#8011,#8012,#8013,#8014,#8015,#8016,#8017,#8018,#8019,#8020,#8021,#8022,
#8023,#8024,#8025,#8026,#8027,#8028,#8029),(#8030,#8031,#8032,#8033,#8034,
#8035,#8036,#8037,#8038,#8039,#8040,#8041,#8042,#8043,#8044,#8045,#8046,
#8047,#8048,#8049,#8050,#8051,#8052,#8053,#8054,#8055,#8056,#8057,#8058,
#8059,#8060,#8061,#8062,#8063,#8064,#8065,#8066,#8067,#8068,#8069,#8070,
#8071,#8072,#8073,#8074,#8075,#8076,#8077,#8078,#8079,#8080,#8081,#8082,
#8083,#8084,#8085,#8086,#8087,#8088,#8089,#8090,#8091,#8092,#8093,#8094,
#8095,#8096,#8097,#8098,#8099,#8100,#8101,#8102,#8103,#8104,#8105,#8106,
#8107,#8108,#8109,#8110,#8111,#8112,#8113,#8114,#8115,#8116,#8117,#8118,
#8119,#8120,#8121,#8122,#8123,#8124,#8125),(#8126,#8127,#8128,#8129,#8130,
#8131,#8132,#8133,#8134,#8135,#8136,#8137,#8138,#8139,#8140,#8141,#8142,
#8143,#8144,#8145,#8146,#8147,#8148,#8149,#8150,#8151,#8152,#8153,#8154,
#8155,#8156,#8157,#8158,#8159,#8160,#8161,#8162,#8163,#8164,#8165,#8166,
#8167,#8168,#8169,#8170,#8171,#8172,#8173,#8174,#8175,#8176,#8177,#8178,
#8179,#8180,#8181,#8182,#8183,#8184,#8185,#8186,#8187,#8188,#8189,#8190,
#8191,#8192,#8193,#8194,#8195,#8196,#8197,#8198,#8199,#8200,#8201,#8202,
#8203,#8204,#8205,#8206,#8207,#8208,#8209,#8210,#8211,#8212,#8213,#8214,
#8215,#8216,#8217,#8218,#8219,#8220,#8221),(#8222,#8223,#8224,#8225,#8226,
#8227,#8228,#8229,#8230,#8231,#8232,#8233,#8234,#8235,#8236,#8237,#8238,
#8239,#8240,#8241,#8242,#8243,#8244,#8245,#8246,#8247,#8248,#8249,#8250,
#8251,#8252,#8253,#8254,#8255,#8256,#8257,#8258,#8259,#8260,#8261,#8262,
#8263,#8264,#8265,#8266,#8267,#8268,#8269,#8270,#8271,#8272,#8273,#8274,
#8275,#8276,#8277,#8278,#8279,#8280,#8281,#8282,#8283,#8284,#8285,#8286,
#8287,#8288,#8289,#8290,#8291,#8292,#8293,#8294,#8295,#8296,#8297,#8298,
#8299,#8300,#8301,#8302,#8303,#8304,#8305,#8306,#8307,#8308,#8309,#8310,
#8311,#8312,#8313,#8314,#8315,#8316,#8317),(#8318,#8319,#8320,#8321,#8322,
#8323,#8324,#8325,#8326,#8327,#8328,#8329,#8330,#8331,#8332,#8333,#8334,
#8335,#8336,#8337,#8338,#8339,#8340,#8341,#8342,#8343,#8344,#8345,#8346,
#8347,#8348,#8349,#8350,#8351,#8352,#8353,#8354,#8355,#8356,#8357,#8358,
#8359,#8360,#8361,#8362,#8363,#8364,#8365,#8366,#8367,#8368,#8369,#8370,
#8371,#8372,#8373,#8374,#8375,#8376,#8377,#8378,#8379,#8380,#8381,#8382,
#8383,#8384,#8385,#8386,#8387,#8388,#8389,#8390,#8391,#8392,#8393,#8394,
#8395,#8396,#8397,#8398,#8399,#8400,#8401,#8402,#8403,#8404,#8405,#8406,
#8407,#8408,#8409,#8410,#8411,#8412,#8413)),.UNSPECIFIED.,.T.,.F.,.F.,(4,
1,1,1,1,1,1,4),(4,1,1,1,1,1,1,1,1,1,1,1,1,1,1,1,1,1,1,1,1,1,1,1,1,1,1,1,
1,1,1,1,1,1,1,1,1,1,1,1,1,1,1,1,1,1,1,1,1,1,1,1,1,1,1,1,1,1,1,1,1,1,1,1,
1,1,1,1,1,1,1,1,1,1,1,1,1,1,1,1,1,1,1,1,1,1,1,1,1,1,1,1,1,4),(-3.14159265358979,
-2.24399475256414,-1.34639685153848,-0.448798950512828,0.448798950512828,
1.34639685153848,2.24399475256414,3.14159265358979),(0.,0.00892857142857143,
0.0178571428571429,0.0267857142857143,0.0357142857142857,0.0446428571428571,
0.0535714285714286,0.0625,0.0714285714285714,0.0803571428571428,0.0892857142857143,
0.107142857142857,0.125,0.133928571428571,0.142857142857143,0.158730158730159,
0.174603174603175,0.19047619047619,0.202380952380952,0.214285714285714,
0.226190476190476,0.238095238095238,0.25,0.261904761904762,0.273809523809524,
0.285714285714286,0.297619047619048,0.30952380952381,0.321428571428571,
0.333333333333333,0.345238095238095,0.357142857142857,0.369047619047619,
0.375,0.380952380952381,0.392857142857143,0.404761904761905,0.416666666666667,
0.428571428571429,0.4375,0.446428571428571,0.455357142857143,0.464285714285714,
0.476190476190476,0.488095238095238,0.5,0.508928571428571,0.517857142857143,
0.535714285714286,0.553571428571429,0.571428571428571,0.580357142857143,
0.589285714285714,0.598214285714286,0.607142857142857,0.616071428571429,
0.625,0.633928571428571,0.642857142857143,0.654761904761905,0.666666666666667,
0.678571428571428,0.6875,0.696428571428571,0.705357142857143,0.714285714285714,
0.726190476190476,0.738095238095238,0.75,0.761904761904762,0.773809523809524,
0.785714285714286,0.797619047619047,0.809523809523809,0.821428571428571,
0.833333333333333,0.845238095238095,0.857142857142857,0.866071428571429,
0.875,0.883928571428571,0.892857142857143,0.901785714285714,0.910714285714286,
0.919642857142857,0.928571428571429,0.9375,0.946428571428571,0.955357142857143,
0.964285714285714,0.973214285714286,0.982142857142857,0.991071428571429,
1.),.UNSPECIFIED.);
#234=B_SPLINE_CURVE_WITH_KNOTS('',3,(#7309,#7310,#7311,#7312,#7313,#7314,
#7315,#7316,#7317,#7318,#7319,#7320,#7321,#7322),.UNSPECIFIED.,.F.,.F.,
(4,2,2,2,2,2,4),(0.714680326757343,0.792648662700719,0.871912238073926,
0.951175813447133,1.03043938882034,1.10970296419355,1.18767130013692),
 .UNSPECIFIED.);
#235=B_SPLINE_CURVE_WITH_KNOTS('',3,(#7326,#7327,#7328,#7329,#7330,#7331,
#7332,#7333),.UNSPECIFIED.,.F.,.F.,(4,2,2,4),(0.317058604482378,0.396322179855585,
0.475585755228792,0.55355409117217),.UNSPECIFIED.);
#236=B_SPLINE_CURVE_WITH_KNOTS('',3,(#7337,#7338,#7339,#7340,#7341,#7342,
#7343,#7344,#7345,#7346,#7347,#7348,#7349,#7350,#7351,#7352,#7353,#7354,
#7355,#7356,#7357,#7358,#7359,#7360,#7361,#7362),.UNSPECIFIED.,.F.,.F.,
(4,2,2,2,2,2,2,2,2,2,2,2,4),(0.,0.0791819055472369,0.158363811094474,0.237545215630596,
0.316726620166718,0.395908024702839,0.475089429238961,0.554271334786198,
0.633453240333435,0.712635145880672,0.791817051427909,0.870998455964031,
0.950179860500153),.UNSPECIFIED.);
#237=B_SPLINE_CURVE_WITH_KNOTS('',3,(#7363,#7364,#7365,#7366,#7367,#7368,
#7369,#7370,#7371,#7372),.UNSPECIFIED.,.F.,.F.,(4,2,2,2,4),(0.950179860500153,
1.02936126503627,1.1085426695724,1.18772457511963,1.26690648066687),
 .UNSPECIFIED.);
#238=B_SPLINE_CURVE_WITH_KNOTS('',3,(#7373,#7374,#7375,#7376,#7377,#7378,
#7379,#7380),.UNSPECIFIED.,.F.,.F.,(4,2,2,4),(0.0805631177925868,0.158531453735964,
0.237795029109171,0.317058604482378),.UNSPECIFIED.);
#239=B_SPLINE_CURVE_WITH_KNOTS('',3,(#8417,#8418,#8419,#8420,#8421,#8422,
#8423,#8424,#8425,#8426,#8427,#8428,#8429,#8430,#8431,#8432,#8433,#8434,
#8435,#8436,#8437,#8438,#8439,#8440,#8441,#8442,#8443,#8444,#8445,#8446,
#8447,#8448,#8449,#8450,#8451,#8452,#8453,#8454,#8455,#8456,#8457,#8458,
#8459,#8460,#8461,#8462,#8463,#8464,#8465,#8466,#8467,#8468,#8469,#8470,
#8471,#8472,#8473,#8474,#8475,#8476,#8477,#8478,#8479,#8480,#8481,#8482,
#8483,#8484,#8485,#8486,#8487,#8488,#8489,#8490,#8491,#8492,#8493,#8494,
#8495,#8496,#8497,#8498,#8499,#8500,#8501,#8502,#8503,#8504,#8505,#8506,
#8507,#8508,#8509,#8510,#8511,#8512),.UNSPECIFIED.,.F.,.F.,(4,1,1,1,1,1,
1,1,1,1,1,1,1,1,1,1,1,1,1,1,1,1,1,1,1,1,1,1,1,1,1,1,1,1,1,1,1,1,1,1,1,1,
1,1,1,1,1,1,1,1,1,1,1,1,1,1,1,1,1,1,1,1,1,1,1,1,1,1,1,1,1,1,1,1,1,1,1,1,
1,1,1,1,1,1,1,1,1,1,1,1,1,1,1,4),(0.,0.00892857142857143,0.0178571428571429,
0.0267857142857143,0.0357142857142857,0.0446428571428571,0.0535714285714286,
0.0625,0.0714285714285714,0.0803571428571428,0.0892857142857143,0.107142857142857,
0.125,0.133928571428571,0.142857142857143,0.158730158730159,0.174603174603175,
0.19047619047619,0.202380952380952,0.214285714285714,0.226190476190476,
0.238095238095238,0.25,0.261904761904762,0.273809523809524,0.285714285714286,
0.297619047619048,0.30952380952381,0.321428571428571,0.333333333333333,
0.345238095238095,0.357142857142857,0.369047619047619,0.375,0.380952380952381,
0.392857142857143,0.404761904761905,0.416666666666667,0.428571428571429,
0.4375,0.446428571428571,0.455357142857143,0.464285714285714,0.476190476190476,
0.488095238095238,0.5,0.508928571428571,0.517857142857143,0.535714285714286,
0.553571428571429,0.571428571428571,0.580357142857143,0.589285714285714,
0.598214285714286,0.607142857142857,0.616071428571429,0.625,0.633928571428571,
0.642857142857143,0.654761904761905,0.666666666666667,0.678571428571428,
0.6875,0.696428571428571,0.705357142857143,0.714285714285714,0.726190476190476,
0.738095238095238,0.75,0.761904761904762,0.773809523809524,0.785714285714286,
0.797619047619047,0.809523809523809,0.821428571428571,0.833333333333333,
0.845238095238095,0.857142857142857,0.866071428571429,0.875,0.883928571428571,
0.892857142857143,0.901785714285714,0.910714285714286,0.919642857142857,
0.928571428571429,0.9375,0.946428571428571,0.955357142857143,0.964285714285714,
0.973214285714286,0.982142857142857,0.991071428571429,1.),.UNSPECIFIED.);
#240=B_SPLINE_CURVE_WITH_KNOTS('',3,(#8709,#8710,#8711,#8712,#8713,#8714,
#8715,#8716,#8717,#8718,#8719,#8720,#8721,#8722,#8723,#8724,#8725,#8726,
#8727,#8728,#8729,#8730),.UNSPECIFIED.,.F.,.F.,(4,2,2,2,2,2,2,2,2,2,4),
(0.0789043916784349,0.21052649634152,0.31578974451228,0.421052992683041,
0.522171766675512,0.623290540667983,0.724409314660453,0.825528088652924,
0.930791336823684,1.03605458499444,1.16767668965753),.UNSPECIFIED.);
#241=B_SPLINE_CURVE_WITH_KNOTS('',3,(#8734,#8735,#8736,#8737,#8738,#8739,
#8740,#8741,#8742,#8743,#8744,#8745,#8746,#8747,#8748,#8749,#8750,#8751,
#8752,#8753,#8754,#8755),.UNSPECIFIED.,.F.,.F.,(4,2,2,2,2,2,2,2,2,2,4),
(0.0774711646211702,0.142095081356994,0.284190162713987,0.410912155766437,
0.514012992401139,0.617113829035841,0.720214665670543,0.823315502305246,
0.950037495357694,1.09213257671469,1.15675649345051),.UNSPECIFIED.);
#242=B_SPLINE_CURVE_WITH_KNOTS('',3,(#8761,#8762,#8763,#8764,#8765,#8766,
#8767,#8768,#8769,#8770,#8771,#8772,#8773,#8774,#8775,#8776,#8777,#8778,
#8779,#8780,#8781,#8782),.UNSPECIFIED.,.F.,.F.,(4,2,2,2,2,2,2,2,2,2,4),
(0.0774711646211703,0.142095081356994,0.284190162713988,0.410912155766436,
0.514012992401139,0.617113829035841,0.720214665670544,0.823315502305246,
0.950037495357695,1.09213257671469,1.15675649345051),.UNSPECIFIED.);
#243=B_SPLINE_CURVE_WITH_KNOTS('',3,(#8786,#8787,#8788,#8789,#8790,#8791,
#8792,#8793,#8794,#8795,#8796,#8797,#8798,#8799,#8800,#8801,#8802,#8803,
#8804,#8805,#8806,#8807),.UNSPECIFIED.,.F.,.F.,(4,2,2,2,2,2,2,2,2,2,4),
(0.0774711646211702,0.142095081356994,0.284190162713988,0.410912155766436,
0.514012992401139,0.617113829035841,0.720214665670544,0.823315502305246,
0.950037495357695,1.09213257671469,1.15675649345051),.UNSPECIFIED.);
#244=B_SPLINE_CURVE_WITH_KNOTS('',3,(#8811,#8812,#8813,#8814,#8815,#8816,
#8817,#8818,#8819,#8820,#8821,#8822,#8823,#8824,#8825,#8826,#8827,#8828,
#8829,#8830,#8831,#8832),.UNSPECIFIED.,.F.,.F.,(4,2,2,2,2,2,2,2,2,2,4),
(0.0774711646211702,0.142095081356994,0.284190162713988,0.410912155766436,
0.514012992401139,0.617113829035842,0.720214665670544,0.823315502305246,
0.950037495357696,1.09213257671469,1.15675649345051),.UNSPECIFIED.);
#245=B_SPLINE_CURVE_WITH_KNOTS('',3,(#8841,#8842,#8843,#8844,#8845,#8846,
#8847,#8848,#8849,#8850,#8851,#8852,#8853,#8854,#8855,#8856,#8857,#8858,
#8859,#8860,#8861,#8862),.UNSPECIFIED.,.F.,.F.,(4,2,2,2,2,2,2,2,2,2,4),
(0.0774711646211702,0.142095081356994,0.284190162713987,0.410912155766436,
0.514012992401139,0.617113829035841,0.720214665670543,0.823315502305246,
0.950037495357695,1.09213257671469,1.15675649345051),.UNSPECIFIED.);
#246=B_SPLINE_CURVE_WITH_KNOTS('',3,(#8866,#8867,#8868,#8869,#8870,#8871,
#8872,#8873,#8874,#8875,#8876,#8877,#8878,#8879,#8880,#8881,#8882,#8883,
#8884,#8885,#8886,#8887),.UNSPECIFIED.,.F.,.F.,(4,2,2,2,2,2,2,2,2,2,4),
(0.0774711646211702,0.142095081356994,0.284190162713987,0.410912155766436,
0.514012992401139,0.617113829035841,0.720214665670543,0.823315502305246,
0.950037495357695,1.09213257671469,1.15675649345051),.UNSPECIFIED.);
#247=B_SPLINE_CURVE_WITH_KNOTS('',3,(#8891,#8892,#8893,#8894,#8895,#8896,
#8897,#8898,#8899,#8900,#8901,#8902,#8903,#8904,#8905,#8906,#8907,#8908,
#8909,#8910,#8911,#8912),.UNSPECIFIED.,.F.,.F.,(4,2,2,2,2,2,2,2,2,2,4),
(0.0774711646211703,0.142095081356994,0.284190162713988,0.410912155766437,
0.514012992401139,0.617113829035841,0.720214665670544,0.823315502305247,
0.950037495357696,1.09213257671469,1.15675649345051),.UNSPECIFIED.);
#248=B_SPLINE_CURVE_WITH_KNOTS('',3,(#8916,#8917,#8918,#8919,#8920,#8921,
#8922,#8923,#8924,#8925,#8926,#8927,#8928,#8929,#8930,#8931,#8932,#8933,
#8934,#8935,#8936,#8937),.UNSPECIFIED.,.F.,.F.,(4,2,2,2,2,2,2,2,2,2,4),
(0.0774711646211703,0.142095081356994,0.284190162713987,0.410912155766436,
0.514012992401139,0.617113829035841,0.720214665670543,0.823315502305245,
0.950037495357694,1.09213257671469,1.15675649345051),.UNSPECIFIED.);
#249=B_SPLINE_CURVE_WITH_KNOTS('',3,(#8941,#8942,#8943,#8944,#8945,#8946,
#8947,#8948,#8949,#8950,#8951,#8952,#8953,#8954,#8955,#8956,#8957,#8958,
#8959,#8960,#8961,#8962),.UNSPECIFIED.,.F.,.F.,(4,2,2,2,2,2,2,2,2,2,4),
(0.0774711646211703,0.142095081356994,0.284190162713988,0.410912155766437,
0.514012992401139,0.617113829035841,0.720214665670544,0.823315502305246,
0.950037495357695,1.09213257671469,1.15675649345051),.UNSPECIFIED.);
#250=B_SPLINE_CURVE_WITH_KNOTS('',3,(#8970,#8971,#8972,#8973,#8974,#8975,
#8976,#8977,#8978,#8979,#8980,#8981,#8982,#8983,#8984,#8985,#8986,#8987,
#8988,#8989,#8990,#8991),.UNSPECIFIED.,.F.,.F.,(4,2,2,2,2,2,2,2,2,2,4),
(0.0789043916784349,0.21052649634152,0.315789744512281,0.421052992683041,
0.522171766675512,0.623290540667983,0.724409314660453,0.825528088652924,
0.930791336823684,1.03605458499444,1.16767668965753),.UNSPECIFIED.);
#251=B_SPLINE_CURVE_WITH_KNOTS('',3,(#8999,#9000,#9001,#9002,#9003,#9004,
#9005,#9006,#9007,#9008,#9009,#9010,#9011,#9012,#9013,#9014,#9015,#9016,
#9017,#9018,#9019,#9020),.UNSPECIFIED.,.F.,.F.,(4,2,2,2,2,2,2,2,2,2,4),
(0.0789043916784348,0.210526496341521,0.315789744512281,0.421052992683042,
0.522171766675513,0.623290540667983,0.724409314660454,0.825528088652925,
0.930791336823685,1.03605458499444,1.16767668965753),.UNSPECIFIED.);
#252=B_SPLINE_CURVE_WITH_KNOTS('',3,(#9028,#9029,#9030,#9031,#9032,#9033,
#9034,#9035,#9036,#9037,#9038,#9039,#9040,#9041,#9042,#9043,#9044,#9045,
#9046,#9047,#9048,#9049),.UNSPECIFIED.,.F.,.F.,(4,2,2,2,2,2,2,2,2,2,4),
(0.0789043916784349,0.21052649634152,0.31578974451228,0.421052992683041,
0.522171766675511,0.623290540667982,0.724409314660453,0.825528088652924,
0.930791336823685,1.03605458499444,1.16767668965753),.UNSPECIFIED.);
#253=B_SPLINE_CURVE_WITH_KNOTS('',3,(#9059,#9060,#9061,#9062,#9063,#9064,
#9065,#9066,#9067,#9068,#9069,#9070,#9071,#9072,#9073,#9074,#9075,#9076,
#9077,#9078,#9079,#9080),.UNSPECIFIED.,.F.,.F.,(4,2,2,2,2,2,2,2,2,2,4),
(0.0789043916784348,0.21052649634152,0.315789744512281,0.421052992683041,
0.522171766675511,0.623290540667982,0.724409314660453,0.825528088652924,
0.930791336823684,1.03605458499444,1.16767668965753),.UNSPECIFIED.);
#254=B_SPLINE_CURVE_WITH_KNOTS('',3,(#9088,#9089,#9090,#9091,#9092,#9093,
#9094,#9095,#9096,#9097,#9098,#9099,#9100,#9101,#9102,#9103,#9104,#9105,
#9106,#9107,#9108,#9109),.UNSPECIFIED.,.F.,.F.,(4,2,2,2,2,2,2,2,2,2,4),
(0.0789043916784348,0.21052649634152,0.31578974451228,0.42105299268304,
0.522171766675511,0.623290540667982,0.724409314660453,0.825528088652924,
0.930791336823684,1.03605458499444,1.16767668965753),.UNSPECIFIED.);
#255=B_SPLINE_CURVE_WITH_KNOTS('',3,(#9117,#9118,#9119,#9120,#9121,#9122,
#9123,#9124,#9125,#9126,#9127,#9128,#9129,#9130,#9131,#9132,#9133,#9134,
#9135,#9136,#9137,#9138),.UNSPECIFIED.,.F.,.F.,(4,2,2,2,2,2,2,2,2,2,4),
(0.0789043916784348,0.21052649634152,0.315789744512281,0.421052992683041,
0.522171766675512,0.623290540667982,0.724409314660453,0.825528088652924,
0.930791336823684,1.03605458499444,1.16767668965753),.UNSPECIFIED.);
#256=B_SPLINE_CURVE_WITH_KNOTS('',3,(#9146,#9147,#9148,#9149,#9150,#9151,
#9152,#9153,#9154,#9155,#9156,#9157,#9158,#9159,#9160,#9161,#9162,#9163,
#9164,#9165,#9166,#9167),.UNSPECIFIED.,.F.,.F.,(4,2,2,2,2,2,2,2,2,2,4),
(0.0789043916784349,0.21052649634152,0.31578974451228,0.42105299268304,
0.522171766675511,0.623290540667982,0.724409314660453,0.825528088652924,
0.930791336823684,1.03605458499444,1.16767668965753),.UNSPECIFIED.);
#257=B_SPLINE_CURVE_WITH_KNOTS('',3,(#9176,#9177,#9178,#9179,#9180,#9181,
#9182,#9183,#9184,#9185,#9186,#9187,#9188,#9189,#9190,#9191,#9192,#9193,
#9194,#9195,#9196,#9197),.UNSPECIFIED.,.F.,.F.,(4,2,2,2,2,2,2,2,2,2,4),
(0.0789043916784348,0.21052649634152,0.31578974451228,0.42105299268304,
0.522171766675511,0.623290540667982,0.724409314660453,0.825528088652924,
0.930791336823684,1.03605458499444,1.16767668965753),.UNSPECIFIED.);
#258=B_SPLINE_CURVE_WITH_KNOTS('',3,(#9823,#9824,#9825,#9826,#9827,#9828),
 .UNSPECIFIED.,.F.,.F.,(4,2,4),(0.917424161667463,0.994436039000116,1.07144791633277),
 .UNSPECIFIED.);
#259=B_SPLINE_CURVE_WITH_KNOTS('',3,(#9832,#9833,#9834,#9835),
 .UNSPECIFIED.,.F.,.F.,(4,4),(0.331478679666705,0.408490556999359),
 .UNSPECIFIED.);
#260=B_SPLINE_CURVE_WITH_KNOTS('',3,(#9839,#9840,#9841,#9842,#9843,#9844,
#9845,#9846,#9847,#9848,#9849,#9850,#9851,#9852,#9853,#9854,#9855,#9856,
#9857,#9858,#9859,#9860,#9861,#9862,#9863,#9864),.UNSPECIFIED.,.F.,.F.,
(4,2,2,2,2,2,2,2,2,2,2,2,4),(0.,0.0792812130427881,0.158562426085576,0.237841058284634,
0.317119690483691,0.396398322682749,0.475676954881806,0.554958167924595,
0.634239380967383,0.713520594010171,0.792801807052959,0.872080439252016,
0.951359071451074),.UNSPECIFIED.);
#261=B_SPLINE_CURVE_WITH_KNOTS('',3,(#9865,#9866,#9867,#9868,#9869,#9870,
#9871,#9872,#9873,#9874),.UNSPECIFIED.,.F.,.F.,(4,2,2,2,4),(0.951359071451074,
1.03063770365013,1.10991633584919,1.18919754889198,1.26847876193477),
 .UNSPECIFIED.);
#262=B_SPLINE_CURVE_WITH_KNOTS('',3,(#9875,#9876,#9877,#9878),
 .UNSPECIFIED.,.F.,.F.,(4,4),(0.254466802334052,0.331478679666705),
 .UNSPECIFIED.);
#263=SHAPE_REPRESENTATION_RELATIONSHIP('SRR','None',#10137,#290);
#264=SHAPE_REPRESENTATION_RELATIONSHIP('SRR','None',#10138,#291);
#265=SHAPE_REPRESENTATION_RELATIONSHIP('SRR','None',#10139,#292);
#266=SHAPE_REPRESENTATION_RELATIONSHIP('SRR','None',#10140,#293);
#267=SHAPE_REPRESENTATION_RELATIONSHIP('SRR','None',#10141,#294);
#268=SHAPE_REPRESENTATION_RELATIONSHIP('SRR','None',#10142,#295);
#269=SHAPE_REPRESENTATION_RELATIONSHIP('SRR','None',#10143,#296);
#270=SHAPE_REPRESENTATION_RELATIONSHIP('SRR','None',#10144,#297);
#271=SHAPE_REPRESENTATION_RELATIONSHIP('SRR','None',#10145,#298);
#272=SHAPE_REPRESENTATION_RELATIONSHIP('SRR','None',#10146,#299);
#273=SHAPE_REPRESENTATION_RELATIONSHIP('SRR','None',#10147,#300);
#274=SHAPE_REPRESENTATION_RELATIONSHIP('SRR','None',#10148,#301);
#275=SHAPE_REPRESENTATION_RELATIONSHIP('SRR','None',#10149,#302);
#276=SHAPE_REPRESENTATION_RELATIONSHIP('SRR','None',#10151,#303);
#277=SHAPE_REPRESENTATION_RELATIONSHIP('SRR','None',#10152,#304);
#278=SHAPE_REPRESENTATION_RELATIONSHIP('SRR','None',#10153,#305);
#279=SHAPE_REPRESENTATION_RELATIONSHIP('SRR','None',#10154,#306);
#280=SHAPE_REPRESENTATION_RELATIONSHIP('SRR','None',#10155,#307);
#281=SHAPE_REPRESENTATION_RELATIONSHIP('SRR','None',#10156,#308);
#282=SHAPE_REPRESENTATION_RELATIONSHIP('SRR','None',#10158,#309);
#283=SHAPE_REPRESENTATION_RELATIONSHIP('SRR','None',#10159,#310);
#284=SHAPE_REPRESENTATION_RELATIONSHIP('SRR','None',#10160,#311);
#285=SHAPE_REPRESENTATION_RELATIONSHIP('SRR','None',#10161,#312);
#286=SHAPE_REPRESENTATION_RELATIONSHIP('SRR','None',#10162,#313);
#287=SHAPE_REPRESENTATION_RELATIONSHIP('SRR','None',#10164,#314);
#288=SHAPE_REPRESENTATION_RELATIONSHIP('SRR','None',#10165,#315);
#289=SHAPE_REPRESENTATION_RELATIONSHIP('SRR','None',#10166,#316);
#290=ADVANCED_BREP_SHAPE_REPRESENTATION('',(#353),#9990);
#291=ADVANCED_BREP_SHAPE_REPRESENTATION('',(#354),#9991);
#292=ADVANCED_BREP_SHAPE_REPRESENTATION('',(#355),#9992);
#293=ADVANCED_BREP_SHAPE_REPRESENTATION('',(#356),#9993);
#294=ADVANCED_BREP_SHAPE_REPRESENTATION('',(#357),#9994);
#295=ADVANCED_BREP_SHAPE_REPRESENTATION('',(#358),#9995);
#296=ADVANCED_BREP_SHAPE_REPRESENTATION('',(#359),#9996);
#297=ADVANCED_BREP_SHAPE_REPRESENTATION('',(#360),#9997);
#298=ADVANCED_BREP_SHAPE_REPRESENTATION('',(#361),#9998);
#299=ADVANCED_BREP_SHAPE_REPRESENTATION('',(#362),#9999);
#300=ADVANCED_BREP_SHAPE_REPRESENTATION('',(#363),#10000);
#301=ADVANCED_BREP_SHAPE_REPRESENTATION('',(#364),#10001);
#302=ADVANCED_BREP_SHAPE_REPRESENTATION('',(#231),#10002);
#303=ADVANCED_BREP_SHAPE_REPRESENTATION('',(#365),#10004);
#304=ADVANCED_BREP_SHAPE_REPRESENTATION('',(#366),#10005);
#305=ADVANCED_BREP_SHAPE_REPRESENTATION('',(#367,#368,#369,#370,#371,#372,
#373,#374,#375),#10006);
#306=ADVANCED_BREP_SHAPE_REPRESENTATION('',(#376),#10007);
#307=ADVANCED_BREP_SHAPE_REPRESENTATION('',(#377,#378),#10008);
#308=ADVANCED_BREP_SHAPE_REPRESENTATION('',(#379),#10009);
#309=ADVANCED_BREP_SHAPE_REPRESENTATION('',(#380),#10011);
#310=ADVANCED_BREP_SHAPE_REPRESENTATION('',(#381),#10012);
#311=ADVANCED_BREP_SHAPE_REPRESENTATION('',(#382),#10013);
#312=ADVANCED_BREP_SHAPE_REPRESENTATION('',(#383),#10014);
#313=ADVANCED_BREP_SHAPE_REPRESENTATION('',(#232),#10015);
#314=ADVANCED_BREP_SHAPE_REPRESENTATION('',(#384),#10017);
#315=ADVANCED_BREP_SHAPE_REPRESENTATION('',(#385),#10018);
#316=ADVANCED_BREP_SHAPE_REPRESENTATION('',(#386),#10019);
#317=STYLED_ITEM('',(#10347),#353);
#318=STYLED_ITEM('',(#10382),#354);
#319=STYLED_ITEM('',(#10382),#355);
#320=STYLED_ITEM('',(#10382),#356);
#321=STYLED_ITEM('',(#10382),#357);
#322=STYLED_ITEM('',(#10361),#358);
#323=STYLED_ITEM('',(#10368),#359);
#324=STYLED_ITEM('',(#10361),#360);
#325=STYLED_ITEM('',(#10354),#361);
#326=STYLED_ITEM('',(#10347),#362);
#327=STYLED_ITEM('',(#10368),#363);
#328=STYLED_ITEM('',(#10375),#364);
#329=STYLED_ITEM('',(#10375),#231);
#330=STYLED_ITEM('',(#10368),#365);
#331=STYLED_ITEM('',(#10368),#366);
#332=STYLED_ITEM('',(#10368),#367);
#333=STYLED_ITEM('',(#10368),#368);
#334=STYLED_ITEM('',(#10368),#369);
#335=STYLED_ITEM('',(#10368),#370);
#336=STYLED_ITEM('',(#10368),#371);
#337=STYLED_ITEM('',(#10368),#372);
#338=STYLED_ITEM('',(#10368),#373);
#339=STYLED_ITEM('',(#10368),#374);
#340=STYLED_ITEM('',(#10368),#375);
#341=STYLED_ITEM('',(#10368),#376);
#342=STYLED_ITEM('',(#10368),#377);
#343=STYLED_ITEM('',(#10368),#378);
#344=STYLED_ITEM('',(#10375),#379);
#345=STYLED_ITEM('',(#10382),#380);
#346=STYLED_ITEM('',(#10368),#381);
#347=STYLED_ITEM('',(#10368),#382);
#348=STYLED_ITEM('',(#10354),#383);
#349=STYLED_ITEM('',(#10375),#232);
#350=STYLED_ITEM('',(#10368),#384);
#351=STYLED_ITEM('',(#10354),#385);
#352=STYLED_ITEM('',(#10375),#386);
#353=MANIFOLD_SOLID_BREP('Body1',#4571);
#354=MANIFOLD_SOLID_BREP('Body1',#4572);
#355=MANIFOLD_SOLID_BREP('Body1',#4573);
#356=MANIFOLD_SOLID_BREP('Body1',#4574);
#357=MANIFOLD_SOLID_BREP('Body1',#4575);
#358=MANIFOLD_SOLID_BREP('Body1',#4576);
#359=MANIFOLD_SOLID_BREP('Body1',#4577);
#360=MANIFOLD_SOLID_BREP('Body1',#4578);
#361=MANIFOLD_SOLID_BREP('Body1',#4579);
#362=MANIFOLD_SOLID_BREP('Body1',#4580);
#363=MANIFOLD_SOLID_BREP('Body1',#4581);
#364=MANIFOLD_SOLID_BREP('Body1',#4582);
#365=MANIFOLD_SOLID_BREP('Body1',#4585);
#366=MANIFOLD_SOLID_BREP('Body1',#4586);
#367=MANIFOLD_SOLID_BREP('Body1',#4587);
#368=MANIFOLD_SOLID_BREP('Body2',#4588);
#369=MANIFOLD_SOLID_BREP('Body3',#4589);
#370=MANIFOLD_SOLID_BREP('Body4',#4590);
#371=MANIFOLD_SOLID_BREP('Body5',#4591);
#372=MANIFOLD_SOLID_BREP('Body6',#4592);
#373=MANIFOLD_SOLID_BREP('Body7',#4593);
#374=MANIFOLD_SOLID_BREP('Body8',#4594);
#375=MANIFOLD_SOLID_BREP('Body9',#4595);
#376=MANIFOLD_SOLID_BREP('Continuous crown cage',#4596);
#377=MANIFOLD_SOLID_BREP('Body1',#4597);
#378=MANIFOLD_SOLID_BREP('Body2',#4598);
#379=MANIFOLD_SOLID_BREP('Body1',#4599);
#380=MANIFOLD_SOLID_BREP('Body1',#4600);
#381=MANIFOLD_SOLID_BREP('Body1',#4601);
#382=MANIFOLD_SOLID_BREP('Body1',#4602);
#383=MANIFOLD_SOLID_BREP('Body1',#4603);
#384=MANIFOLD_SOLID_BREP('Body1',#4606);
#385=MANIFOLD_SOLID_BREP('Body1',#4607);
#386=MANIFOLD_SOLID_BREP('Body1',#4608);
#387=FACE_BOUND('',#968,.T.);
#388=FACE_BOUND('',#969,.T.);
#389=FACE_BOUND('',#970,.T.);
#390=FACE_BOUND('',#971,.T.);
#391=FACE_BOUND('',#972,.T.);
#392=FACE_BOUND('',#973,.T.);
#393=FACE_BOUND('',#974,.T.);
#394=FACE_BOUND('',#976,.T.);
#395=FACE_BOUND('',#977,.T.);
#396=FACE_BOUND('',#978,.T.);
#397=FACE_BOUND('',#979,.T.);
#398=FACE_BOUND('',#980,.T.);
#399=FACE_BOUND('',#981,.T.);
#400=FACE_BOUND('',#982,.T.);
#401=FACE_BOUND('',#1000,.T.);
#402=FACE_BOUND('',#1002,.T.);
#403=FACE_BOUND('',#1006,.T.);
#404=FACE_BOUND('',#1007,.T.);
#405=FACE_BOUND('',#1008,.T.);
#406=FACE_BOUND('',#1009,.T.);
#407=FACE_BOUND('',#1010,.T.);
#408=FACE_BOUND('',#1015,.T.);
#409=FACE_BOUND('',#1016,.T.);
#410=FACE_BOUND('',#1017,.T.);
#411=FACE_BOUND('',#1018,.T.);
#412=FACE_BOUND('',#1022,.T.);
#413=FACE_BOUND('',#1024,.T.);
#414=FACE_BOUND('',#1029,.T.);
#415=FACE_BOUND('',#1031,.T.);
#416=FACE_BOUND('',#1033,.T.);
#417=FACE_BOUND('',#1035,.T.);
#418=FACE_BOUND('',#1040,.T.);
#419=FACE_BOUND('',#1044,.T.);
#420=FACE_BOUND('',#1045,.T.);
#421=FACE_BOUND('',#1046,.T.);
#422=FACE_BOUND('',#1048,.T.);
#423=FACE_BOUND('',#1049,.T.);
#424=FACE_BOUND('',#1050,.T.);
#425=FACE_BOUND('',#1053,.T.);
#426=FACE_BOUND('',#1057,.T.);
#427=FACE_BOUND('',#1059,.T.);
#428=FACE_BOUND('',#1066,.T.);
#429=FACE_BOUND('',#1068,.T.);
#430=FACE_BOUND('',#1083,.T.);
#431=FACE_BOUND('',#1091,.T.);
#432=FACE_BOUND('',#1094,.T.);
#433=FACE_BOUND('',#1099,.T.);
#434=FACE_BOUND('',#1104,.T.);
#435=FACE_BOUND('',#1135,.T.);
#436=FACE_BOUND('',#1138,.T.);
#437=FACE_BOUND('',#1141,.T.);
#438=FACE_BOUND('',#1144,.T.);
#439=FACE_BOUND('',#1147,.T.);
#440=FACE_BOUND('',#1158,.T.);
#441=FACE_BOUND('',#1210,.T.);
#442=FACE_BOUND('',#1213,.T.);
#443=FACE_BOUND('',#1215,.T.);
#444=FACE_BOUND('',#1216,.T.);
#445=FACE_BOUND('',#1217,.T.);
#446=FACE_BOUND('',#1218,.T.);
#447=FACE_BOUND('',#1219,.T.);
#448=FACE_BOUND('',#1220,.T.);
#449=FACE_BOUND('',#1221,.T.);
#450=FACE_BOUND('',#1222,.T.);
#451=FACE_BOUND('',#1223,.T.);
#452=FACE_BOUND('',#1224,.T.);
#453=FACE_BOUND('',#1225,.T.);
#454=FACE_BOUND('',#1226,.T.);
#455=FACE_BOUND('',#1227,.T.);
#456=FACE_BOUND('',#1228,.T.);
#457=FACE_BOUND('',#1229,.T.);
#458=FACE_BOUND('',#1230,.T.);
#459=FACE_BOUND('',#1231,.T.);
#460=FACE_BOUND('',#1232,.T.);
#461=FACE_BOUND('',#1233,.T.);
#462=FACE_BOUND('',#1234,.T.);
#463=FACE_BOUND('',#1235,.T.);
#464=FACE_BOUND('',#1236,.T.);
#465=FACE_BOUND('',#1237,.T.);
#466=FACE_BOUND('',#1238,.T.);
#467=FACE_BOUND('',#1239,.T.);
#468=FACE_BOUND('',#1243,.T.);
#469=FACE_BOUND('',#1244,.T.);
#470=FACE_BOUND('',#1245,.T.);
#471=FACE_BOUND('',#1246,.T.);
#472=FACE_BOUND('',#1247,.T.);
#473=FACE_BOUND('',#1248,.T.);
#474=FACE_BOUND('',#1249,.T.);
#475=FACE_BOUND('',#1250,.T.);
#476=FACE_BOUND('',#1251,.T.);
#477=FACE_BOUND('',#1255,.T.);
#478=FACE_BOUND('',#1256,.T.);
#479=FACE_BOUND('',#1257,.T.);
#480=FACE_BOUND('',#1258,.T.);
#481=FACE_BOUND('',#1259,.T.);
#482=FACE_BOUND('',#1263,.T.);
#483=FACE_BOUND('',#1265,.T.);
#484=FACE_BOUND('',#1272,.T.);
#485=FACE_BOUND('',#1276,.T.);
#486=FACE_BOUND('',#1277,.T.);
#487=FACE_BOUND('',#1278,.T.);
#488=FACE_BOUND('',#1279,.T.);
#489=FACE_BOUND('',#1280,.T.);
#490=FACE_BOUND('',#1282,.T.);
#491=FACE_BOUND('',#1283,.T.);
#492=FACE_BOUND('',#1284,.T.);
#493=FACE_BOUND('',#1285,.T.);
#494=FACE_BOUND('',#1286,.T.);
#495=FACE_BOUND('',#1306,.T.);
#496=FACE_BOUND('',#1307,.T.);
#497=FACE_BOUND('',#1308,.T.);
#498=FACE_BOUND('',#1309,.T.);
#499=FACE_BOUND('',#1310,.T.);
#500=FACE_BOUND('',#1311,.T.);
#501=FACE_BOUND('',#1312,.T.);
#502=FACE_BOUND('',#1313,.T.);
#503=FACE_BOUND('',#1314,.T.);
#504=FACE_BOUND('',#1315,.T.);
#505=FACE_BOUND('',#1316,.T.);
#506=FACE_BOUND('',#1317,.T.);
#507=FACE_BOUND('',#1318,.T.);
#508=FACE_BOUND('',#1319,.T.);
#509=FACE_BOUND('',#1320,.T.);
#510=FACE_BOUND('',#1321,.T.);
#511=FACE_BOUND('',#1322,.T.);
#512=FACE_BOUND('',#1324,.T.);
#513=FACE_BOUND('',#1325,.T.);
#514=FACE_BOUND('',#1326,.T.);
#515=FACE_BOUND('',#1327,.T.);
#516=FACE_BOUND('',#1328,.T.);
#517=FACE_BOUND('',#1329,.T.);
#518=FACE_BOUND('',#1330,.T.);
#519=FACE_BOUND('',#1331,.T.);
#520=FACE_BOUND('',#1332,.T.);
#521=FACE_BOUND('',#1333,.T.);
#522=FACE_BOUND('',#1334,.T.);
#523=FACE_BOUND('',#1335,.T.);
#524=FACE_BOUND('',#1336,.T.);
#525=FACE_BOUND('',#1337,.T.);
#526=FACE_BOUND('',#1338,.T.);
#527=FACE_BOUND('',#1339,.T.);
#528=FACE_BOUND('',#1340,.T.);
#529=FACE_BOUND('',#1346,.T.);
#530=FACE_BOUND('',#1361,.T.);
#531=FACE_BOUND('',#1363,.T.);
#532=FACE_BOUND('',#1372,.T.);
#533=FACE_BOUND('',#1374,.T.);
#534=FACE_BOUND('',#1376,.T.);
#535=FACE_BOUND('',#1378,.T.);
#536=FACE_BOUND('',#1387,.T.);
#537=PLANE('',#4931);
#538=PLANE('',#4932);
#539=PLANE('',#4933);
#540=PLANE('',#4934);
#541=PLANE('',#4935);
#542=PLANE('',#4936);
#543=PLANE('',#4941);
#544=PLANE('',#4942);
#545=PLANE('',#4947);
#546=PLANE('',#4948);
#547=PLANE('',#4953);
#548=PLANE('',#4954);
#549=PLANE('',#4959);
#550=PLANE('',#4960);
#551=PLANE('',#4974);
#552=PLANE('',#4977);
#553=PLANE('',#4983);
#554=PLANE('',#4989);
#555=PLANE('',#4990);
#556=PLANE('',#4998);
#557=PLANE('',#4999);
#558=PLANE('',#5001);
#559=PLANE('',#5005);
#560=PLANE('',#5012);
#561=PLANE('',#5013);
#562=PLANE('',#5024);
#563=PLANE('',#5031);
#564=PLANE('',#5032);
#565=PLANE('',#5037);
#566=PLANE('',#5044);
#567=PLANE('',#5045);
#568=PLANE('',#5049);
#569=PLANE('',#5050);
#570=PLANE('',#5058);
#571=PLANE('',#5059);
#572=PLANE('',#5061);
#573=PLANE('',#5062);
#574=PLANE('',#5063);
#575=PLANE('',#5064);
#576=PLANE('',#5065);
#577=PLANE('',#5066);
#578=PLANE('',#5067);
#579=PLANE('',#5068);
#580=PLANE('',#5069);
#581=PLANE('',#5071);
#582=PLANE('',#5079);
#583=PLANE('',#5099);
#584=PLANE('',#5102);
#585=PLANE('',#5114);
#586=PLANE('',#5123);
#587=PLANE('',#5160);
#588=PLANE('',#5165);
#589=PLANE('',#5170);
#590=PLANE('',#5175);
#591=PLANE('',#5181);
#592=PLANE('',#5186);
#593=PLANE('',#5191);
#594=PLANE('',#5200);
#595=PLANE('',#5204);
#596=PLANE('',#5205);
#597=PLANE('',#5207);
#598=PLANE('',#5212);
#599=PLANE('',#5215);
#600=PLANE('',#5220);
#601=PLANE('',#5229);
#602=PLANE('',#5231);
#603=PLANE('',#5232);
#604=PLANE('',#5233);
#605=PLANE('',#5234);
#606=PLANE('',#5235);
#607=PLANE('',#5236);
#608=PLANE('',#5237);
#609=PLANE('',#5238);
#610=PLANE('',#5248);
#611=PLANE('',#5252);
#612=PLANE('',#5256);
#613=PLANE('',#5260);
#614=PLANE('',#5264);
#615=PLANE('',#5268);
#616=PLANE('',#5272);
#617=PLANE('',#5276);
#618=PLANE('',#5280);
#619=PLANE('',#5284);
#620=PLANE('',#5288);
#621=PLANE('',#5292);
#622=PLANE('',#5296);
#623=PLANE('',#5300);
#624=PLANE('',#5304);
#625=PLANE('',#5308);
#626=PLANE('',#5312);
#627=PLANE('',#5316);
#628=PLANE('',#5320);
#629=PLANE('',#5324);
#630=PLANE('',#5349);
#631=PLANE('',#5354);
#632=PLANE('',#5356);
#633=PLANE('',#5363);
#634=PLANE('',#5368);
#635=PLANE('',#5376);
#636=PLANE('',#5377);
#637=PLANE('',#5394);
#638=PLANE('',#5401);
#639=PLANE('',#5402);
#640=PLANE('',#5458);
#641=PLANE('',#5459);
#642=PLANE('',#5461);
#643=PLANE('',#5469);
#644=PLANE('',#5477);
#645=PLANE('',#5478);
#646=PLANE('',#5479);
#647=PLANE('',#5480);
#648=PLANE('',#5481);
#649=PLANE('',#5482);
#650=PLANE('',#5483);
#651=PLANE('',#5484);
#652=PLANE('',#5485);
#653=PLANE('',#5523);
#654=PLANE('',#5525);
#655=PLANE('',#5528);
#656=PLANE('',#5535);
#657=PLANE('',#5537);
#658=PLANE('',#5541);
#659=PLANE('',#5548);
#660=PLANE('',#5549);
#661=PLANE('',#5551);
#662=PLANE('',#5552);
#663=PLANE('',#5553);
#664=PLANE('',#5554);
#665=PLANE('',#5555);
#666=PLANE('',#5556);
#667=PLANE('',#5557);
#668=PLANE('',#5558);
#669=PLANE('',#5566);
#670=FACE_OUTER_BOUND('',#956,.T.);
#671=FACE_OUTER_BOUND('',#957,.T.);
#672=FACE_OUTER_BOUND('',#958,.T.);
#673=FACE_OUTER_BOUND('',#959,.T.);
#674=FACE_OUTER_BOUND('',#960,.T.);
#675=FACE_OUTER_BOUND('',#961,.T.);
#676=FACE_OUTER_BOUND('',#962,.T.);
#677=FACE_OUTER_BOUND('',#963,.T.);
#678=FACE_OUTER_BOUND('',#964,.T.);
#679=FACE_OUTER_BOUND('',#965,.T.);
#680=FACE_OUTER_BOUND('',#966,.T.);
#681=FACE_OUTER_BOUND('',#967,.T.);
#682=FACE_OUTER_BOUND('',#975,.T.);
#683=FACE_OUTER_BOUND('',#983,.T.);
#684=FACE_OUTER_BOUND('',#984,.T.);
#685=FACE_OUTER_BOUND('',#985,.T.);
#686=FACE_OUTER_BOUND('',#986,.T.);
#687=FACE_OUTER_BOUND('',#987,.T.);
#688=FACE_OUTER_BOUND('',#988,.T.);
#689=FACE_OUTER_BOUND('',#989,.T.);
#690=FACE_OUTER_BOUND('',#990,.T.);
#691=FACE_OUTER_BOUND('',#991,.T.);
#692=FACE_OUTER_BOUND('',#992,.T.);
#693=FACE_OUTER_BOUND('',#993,.T.);
#694=FACE_OUTER_BOUND('',#994,.T.);
#695=FACE_OUTER_BOUND('',#995,.T.);
#696=FACE_OUTER_BOUND('',#996,.T.);
#697=FACE_OUTER_BOUND('',#997,.T.);
#698=FACE_OUTER_BOUND('',#998,.T.);
#699=FACE_OUTER_BOUND('',#999,.T.);
#700=FACE_OUTER_BOUND('',#1001,.T.);
#701=FACE_OUTER_BOUND('',#1003,.T.);
#702=FACE_OUTER_BOUND('',#1004,.T.);
#703=FACE_OUTER_BOUND('',#1005,.T.);
#704=FACE_OUTER_BOUND('',#1011,.T.);
#705=FACE_OUTER_BOUND('',#1012,.T.);
#706=FACE_OUTER_BOUND('',#1013,.T.);
#707=FACE_OUTER_BOUND('',#1014,.T.);
#708=FACE_OUTER_BOUND('',#1019,.T.);
#709=FACE_OUTER_BOUND('',#1020,.T.);
#710=FACE_OUTER_BOUND('',#1021,.T.);
#711=FACE_OUTER_BOUND('',#1023,.T.);
#712=FACE_OUTER_BOUND('',#1025,.T.);
#713=FACE_OUTER_BOUND('',#1026,.T.);
#714=FACE_OUTER_BOUND('',#1027,.T.);
#715=FACE_OUTER_BOUND('',#1028,.T.);
#716=FACE_OUTER_BOUND('',#1030,.T.);
#717=FACE_OUTER_BOUND('',#1032,.T.);
#718=FACE_OUTER_BOUND('',#1034,.T.);
#719=FACE_OUTER_BOUND('',#1036,.T.);
#720=FACE_OUTER_BOUND('',#1037,.T.);
#721=FACE_OUTER_BOUND('',#1038,.T.);
#722=FACE_OUTER_BOUND('',#1039,.T.);
#723=FACE_OUTER_BOUND('',#1041,.T.);
#724=FACE_OUTER_BOUND('',#1042,.T.);
#725=FACE_OUTER_BOUND('',#1043,.T.);
#726=FACE_OUTER_BOUND('',#1047,.T.);
#727=FACE_OUTER_BOUND('',#1051,.T.);
#728=FACE_OUTER_BOUND('',#1052,.T.);
#729=FACE_OUTER_BOUND('',#1054,.T.);
#730=FACE_OUTER_BOUND('',#1055,.T.);
#731=FACE_OUTER_BOUND('',#1056,.T.);
#732=FACE_OUTER_BOUND('',#1058,.T.);
#733=FACE_OUTER_BOUND('',#1060,.T.);
#734=FACE_OUTER_BOUND('',#1061,.T.);
#735=FACE_OUTER_BOUND('',#1062,.T.);
#736=FACE_OUTER_BOUND('',#1063,.T.);
#737=FACE_OUTER_BOUND('',#1064,.T.);
#738=FACE_OUTER_BOUND('',#1065,.T.);
#739=FACE_OUTER_BOUND('',#1067,.T.);
#740=FACE_OUTER_BOUND('',#1069,.T.);
#741=FACE_OUTER_BOUND('',#1070,.T.);
#742=FACE_OUTER_BOUND('',#1071,.T.);
#743=FACE_OUTER_BOUND('',#1072,.T.);
#744=FACE_OUTER_BOUND('',#1073,.T.);
#745=FACE_OUTER_BOUND('',#1074,.T.);
#746=FACE_OUTER_BOUND('',#1075,.T.);
#747=FACE_OUTER_BOUND('',#1076,.T.);
#748=FACE_OUTER_BOUND('',#1077,.T.);
#749=FACE_OUTER_BOUND('',#1078,.T.);
#750=FACE_OUTER_BOUND('',#1079,.T.);
#751=FACE_OUTER_BOUND('',#1080,.T.);
#752=FACE_OUTER_BOUND('',#1081,.T.);
#753=FACE_OUTER_BOUND('',#1082,.T.);
#754=FACE_OUTER_BOUND('',#1084,.T.);
#755=FACE_OUTER_BOUND('',#1085,.T.);
#756=FACE_OUTER_BOUND('',#1086,.T.);
#757=FACE_OUTER_BOUND('',#1087,.T.);
#758=FACE_OUTER_BOUND('',#1088,.T.);
#759=FACE_OUTER_BOUND('',#1089,.T.);
#760=FACE_OUTER_BOUND('',#1090,.T.);
#761=FACE_OUTER_BOUND('',#1092,.T.);
#762=FACE_OUTER_BOUND('',#1093,.T.);
#763=FACE_OUTER_BOUND('',#1095,.T.);
#764=FACE_OUTER_BOUND('',#1096,.T.);
#765=FACE_OUTER_BOUND('',#1097,.T.);
#766=FACE_OUTER_BOUND('',#1098,.T.);
#767=FACE_OUTER_BOUND('',#1100,.T.);
#768=FACE_OUTER_BOUND('',#1101,.T.);
#769=FACE_OUTER_BOUND('',#1102,.T.);
#770=FACE_OUTER_BOUND('',#1103,.T.);
#771=FACE_OUTER_BOUND('',#1105,.T.);
#772=FACE_OUTER_BOUND('',#1106,.T.);
#773=FACE_OUTER_BOUND('',#1107,.T.);
#774=FACE_OUTER_BOUND('',#1108,.T.);
#775=FACE_OUTER_BOUND('',#1109,.T.);
#776=FACE_OUTER_BOUND('',#1110,.T.);
#777=FACE_OUTER_BOUND('',#1111,.T.);
#778=FACE_OUTER_BOUND('',#1112,.T.);
#779=FACE_OUTER_BOUND('',#1113,.T.);
#780=FACE_OUTER_BOUND('',#1114,.T.);
#781=FACE_OUTER_BOUND('',#1115,.T.);
#782=FACE_OUTER_BOUND('',#1116,.T.);
#783=FACE_OUTER_BOUND('',#1117,.T.);
#784=FACE_OUTER_BOUND('',#1118,.T.);
#785=FACE_OUTER_BOUND('',#1119,.T.);
#786=FACE_OUTER_BOUND('',#1120,.T.);
#787=FACE_OUTER_BOUND('',#1121,.T.);
#788=FACE_OUTER_BOUND('',#1122,.T.);
#789=FACE_OUTER_BOUND('',#1123,.T.);
#790=FACE_OUTER_BOUND('',#1124,.T.);
#791=FACE_OUTER_BOUND('',#1125,.T.);
#792=FACE_OUTER_BOUND('',#1126,.T.);
#793=FACE_OUTER_BOUND('',#1127,.T.);
#794=FACE_OUTER_BOUND('',#1128,.T.);
#795=FACE_OUTER_BOUND('',#1129,.T.);
#796=FACE_OUTER_BOUND('',#1130,.T.);
#797=FACE_OUTER_BOUND('',#1131,.T.);
#798=FACE_OUTER_BOUND('',#1132,.T.);
#799=FACE_OUTER_BOUND('',#1133,.T.);
#800=FACE_OUTER_BOUND('',#1134,.T.);
#801=FACE_OUTER_BOUND('',#1136,.T.);
#802=FACE_OUTER_BOUND('',#1137,.T.);
#803=FACE_OUTER_BOUND('',#1139,.T.);
#804=FACE_OUTER_BOUND('',#1140,.T.);
#805=FACE_OUTER_BOUND('',#1142,.T.);
#806=FACE_OUTER_BOUND('',#1143,.T.);
#807=FACE_OUTER_BOUND('',#1145,.T.);
#808=FACE_OUTER_BOUND('',#1146,.T.);
#809=FACE_OUTER_BOUND('',#1148,.T.);
#810=FACE_OUTER_BOUND('',#1149,.T.);
#811=FACE_OUTER_BOUND('',#1150,.T.);
#812=FACE_OUTER_BOUND('',#1151,.T.);
#813=FACE_OUTER_BOUND('',#1152,.T.);
#814=FACE_OUTER_BOUND('',#1153,.T.);
#815=FACE_OUTER_BOUND('',#1154,.T.);
#816=FACE_OUTER_BOUND('',#1155,.T.);
#817=FACE_OUTER_BOUND('',#1156,.T.);
#818=FACE_OUTER_BOUND('',#1157,.T.);
#819=FACE_OUTER_BOUND('',#1159,.T.);
#820=FACE_OUTER_BOUND('',#1160,.T.);
#821=FACE_OUTER_BOUND('',#1161,.T.);
#822=FACE_OUTER_BOUND('',#1162,.T.);
#823=FACE_OUTER_BOUND('',#1163,.T.);
#824=FACE_OUTER_BOUND('',#1164,.T.);
#825=FACE_OUTER_BOUND('',#1165,.T.);
#826=FACE_OUTER_BOUND('',#1166,.T.);
#827=FACE_OUTER_BOUND('',#1167,.T.);
#828=FACE_OUTER_BOUND('',#1168,.T.);
#829=FACE_OUTER_BOUND('',#1169,.T.);
#830=FACE_OUTER_BOUND('',#1170,.T.);
#831=FACE_OUTER_BOUND('',#1171,.T.);
#832=FACE_OUTER_BOUND('',#1172,.T.);
#833=FACE_OUTER_BOUND('',#1173,.T.);
#834=FACE_OUTER_BOUND('',#1174,.T.);
#835=FACE_OUTER_BOUND('',#1175,.T.);
#836=FACE_OUTER_BOUND('',#1176,.T.);
#837=FACE_OUTER_BOUND('',#1177,.T.);
#838=FACE_OUTER_BOUND('',#1178,.T.);
#839=FACE_OUTER_BOUND('',#1179,.T.);
#840=FACE_OUTER_BOUND('',#1180,.T.);
#841=FACE_OUTER_BOUND('',#1181,.T.);
#842=FACE_OUTER_BOUND('',#1182,.T.);
#843=FACE_OUTER_BOUND('',#1183,.T.);
#844=FACE_OUTER_BOUND('',#1184,.T.);
#845=FACE_OUTER_BOUND('',#1185,.T.);
#846=FACE_OUTER_BOUND('',#1186,.T.);
#847=FACE_OUTER_BOUND('',#1187,.T.);
#848=FACE_OUTER_BOUND('',#1188,.T.);
#849=FACE_OUTER_BOUND('',#1189,.T.);
#850=FACE_OUTER_BOUND('',#1190,.T.);
#851=FACE_OUTER_BOUND('',#1191,.T.);
#852=FACE_OUTER_BOUND('',#1192,.T.);
#853=FACE_OUTER_BOUND('',#1193,.T.);
#854=FACE_OUTER_BOUND('',#1194,.T.);
#855=FACE_OUTER_BOUND('',#1195,.T.);
#856=FACE_OUTER_BOUND('',#1196,.T.);
#857=FACE_OUTER_BOUND('',#1197,.T.);
#858=FACE_OUTER_BOUND('',#1198,.T.);
#859=FACE_OUTER_BOUND('',#1199,.T.);
#860=FACE_OUTER_BOUND('',#1200,.T.);
#861=FACE_OUTER_BOUND('',#1201,.T.);
#862=FACE_OUTER_BOUND('',#1202,.T.);
#863=FACE_OUTER_BOUND('',#1203,.T.);
#864=FACE_OUTER_BOUND('',#1204,.T.);
#865=FACE_OUTER_BOUND('',#1205,.T.);
#866=FACE_OUTER_BOUND('',#1206,.T.);
#867=FACE_OUTER_BOUND('',#1207,.T.);
#868=FACE_OUTER_BOUND('',#1208,.T.);
#869=FACE_OUTER_BOUND('',#1209,.T.);
#870=FACE_OUTER_BOUND('',#1211,.T.);
#871=FACE_OUTER_BOUND('',#1212,.T.);
#872=FACE_OUTER_BOUND('',#1214,.T.);
#873=FACE_OUTER_BOUND('',#1240,.T.);
#874=FACE_OUTER_BOUND('',#1241,.T.);
#875=FACE_OUTER_BOUND('',#1242,.T.);
#876=FACE_OUTER_BOUND('',#1252,.T.);
#877=FACE_OUTER_BOUND('',#1253,.T.);
#878=FACE_OUTER_BOUND('',#1254,.T.);
#879=FACE_OUTER_BOUND('',#1260,.T.);
#880=FACE_OUTER_BOUND('',#1261,.T.);
#881=FACE_OUTER_BOUND('',#1262,.T.);
#882=FACE_OUTER_BOUND('',#1264,.T.);
#883=FACE_OUTER_BOUND('',#1266,.T.);
#884=FACE_OUTER_BOUND('',#1267,.T.);
#885=FACE_OUTER_BOUND('',#1268,.T.);
#886=FACE_OUTER_BOUND('',#1269,.T.);
#887=FACE_OUTER_BOUND('',#1270,.T.);
#888=FACE_OUTER_BOUND('',#1271,.T.);
#889=FACE_OUTER_BOUND('',#1273,.T.);
#890=FACE_OUTER_BOUND('',#1274,.T.);
#891=FACE_OUTER_BOUND('',#1275,.T.);
#892=FACE_OUTER_BOUND('',#1281,.T.);
#893=FACE_OUTER_BOUND('',#1287,.T.);
#894=FACE_OUTER_BOUND('',#1288,.T.);
#895=FACE_OUTER_BOUND('',#1289,.T.);
#896=FACE_OUTER_BOUND('',#1290,.T.);
#897=FACE_OUTER_BOUND('',#1291,.T.);
#898=FACE_OUTER_BOUND('',#1292,.T.);
#899=FACE_OUTER_BOUND('',#1293,.T.);
#900=FACE_OUTER_BOUND('',#1294,.T.);
#901=FACE_OUTER_BOUND('',#1295,.T.);
#902=FACE_OUTER_BOUND('',#1296,.T.);
#903=FACE_OUTER_BOUND('',#1297,.T.);
#904=FACE_OUTER_BOUND('',#1298,.T.);
#905=FACE_OUTER_BOUND('',#1299,.T.);
#906=FACE_OUTER_BOUND('',#1300,.T.);
#907=FACE_OUTER_BOUND('',#1301,.T.);
#908=FACE_OUTER_BOUND('',#1302,.T.);
#909=FACE_OUTER_BOUND('',#1303,.T.);
#910=FACE_OUTER_BOUND('',#1304,.T.);
#911=FACE_OUTER_BOUND('',#1305,.T.);
#912=FACE_OUTER_BOUND('',#1323,.T.);
#913=FACE_OUTER_BOUND('',#1341,.T.);
#914=FACE_OUTER_BOUND('',#1342,.T.);
#915=FACE_OUTER_BOUND('',#1343,.T.);
#916=FACE_OUTER_BOUND('',#1344,.T.);
#917=FACE_OUTER_BOUND('',#1345,.T.);
#918=FACE_OUTER_BOUND('',#1347,.T.);
#919=FACE_OUTER_BOUND('',#1348,.T.);
#920=FACE_OUTER_BOUND('',#1349,.T.);
#921=FACE_OUTER_BOUND('',#1350,.T.);
#922=FACE_OUTER_BOUND('',#1351,.T.);
#923=FACE_OUTER_BOUND('',#1352,.T.);
#924=FACE_OUTER_BOUND('',#1353,.T.);
#925=FACE_OUTER_BOUND('',#1354,.T.);
#926=FACE_OUTER_BOUND('',#1355,.T.);
#927=FACE_OUTER_BOUND('',#1356,.T.);
#928=FACE_OUTER_BOUND('',#1357,.T.);
#929=FACE_OUTER_BOUND('',#1358,.T.);
#930=FACE_OUTER_BOUND('',#1359,.T.);
#931=FACE_OUTER_BOUND('',#1360,.T.);
#932=FACE_OUTER_BOUND('',#1362,.T.);
#933=FACE_OUTER_BOUND('',#1364,.T.);
#934=FACE_OUTER_BOUND('',#1365,.T.);
#935=FACE_OUTER_BOUND('',#1366,.T.);
#936=FACE_OUTER_BOUND('',#1367,.T.);
#937=FACE_OUTER_BOUND('',#1368,.T.);
#938=FACE_OUTER_BOUND('',#1369,.T.);
#939=FACE_OUTER_BOUND('',#1370,.T.);
#940=FACE_OUTER_BOUND('',#1371,.T.);
#941=FACE_OUTER_BOUND('',#1373,.T.);
#942=FACE_OUTER_BOUND('',#1375,.T.);
#943=FACE_OUTER_BOUND('',#1377,.T.);
#944=FACE_OUTER_BOUND('',#1379,.T.);
#945=FACE_OUTER_BOUND('',#1380,.T.);
#946=FACE_OUTER_BOUND('',#1381,.T.);
#947=FACE_OUTER_BOUND('',#1382,.T.);
#948=FACE_OUTER_BOUND('',#1383,.T.);
#949=FACE_OUTER_BOUND('',#1384,.T.);
#950=FACE_OUTER_BOUND('',#1385,.T.);
#951=FACE_OUTER_BOUND('',#1386,.T.);
#952=FACE_OUTER_BOUND('',#1388,.T.);
#953=FACE_OUTER_BOUND('',#1389,.T.);
#954=FACE_OUTER_BOUND('',#1390,.T.);
#955=FACE_OUTER_BOUND('',#1391,.T.);
#956=EDGE_LOOP('',(#3063,#3064,#3065,#3066));
#957=EDGE_LOOP('',(#3067,#3068,#3069,#3070));
#958=EDGE_LOOP('',(#3071,#3072,#3073,#3074));
#959=EDGE_LOOP('',(#3075,#3076,#3077,#3078));
#960=EDGE_LOOP('',(#3079,#3080,#3081,#3082));
#961=EDGE_LOOP('',(#3083,#3084,#3085,#3086));
#962=EDGE_LOOP('',(#3087,#3088,#3089,#3090));
#963=EDGE_LOOP('',(#3091,#3092,#3093,#3094));
#964=EDGE_LOOP('',(#3095,#3096,#3097,#3098));
#965=EDGE_LOOP('',(#3099,#3100,#3101,#3102));
#966=EDGE_LOOP('',(#3103,#3104,#3105,#3106));
#967=EDGE_LOOP('',(#3107,#3108,#3109,#3110));
#968=EDGE_LOOP('',(#3111));
#969=EDGE_LOOP('',(#3112));
#970=EDGE_LOOP('',(#3113));
#971=EDGE_LOOP('',(#3114));
#972=EDGE_LOOP('',(#3115));
#973=EDGE_LOOP('',(#3116));
#974=EDGE_LOOP('',(#3117));
#975=EDGE_LOOP('',(#3118,#3119,#3120,#3121));
#976=EDGE_LOOP('',(#3122));
#977=EDGE_LOOP('',(#3123));
#978=EDGE_LOOP('',(#3124));
#979=EDGE_LOOP('',(#3125));
#980=EDGE_LOOP('',(#3126));
#981=EDGE_LOOP('',(#3127));
#982=EDGE_LOOP('',(#3128));
#983=EDGE_LOOP('',(#3129,#3130,#3131,#3132));
#984=EDGE_LOOP('',(#3133));
#985=EDGE_LOOP('',(#3134));
#986=EDGE_LOOP('',(#3135,#3136,#3137,#3138));
#987=EDGE_LOOP('',(#3139));
#988=EDGE_LOOP('',(#3140));
#989=EDGE_LOOP('',(#3141,#3142,#3143,#3144));
#990=EDGE_LOOP('',(#3145));
#991=EDGE_LOOP('',(#3146));
#992=EDGE_LOOP('',(#3147,#3148,#3149,#3150));
#993=EDGE_LOOP('',(#3151));
#994=EDGE_LOOP('',(#3152));
#995=EDGE_LOOP('',(#3153,#3154,#3155,#3156));
#996=EDGE_LOOP('',(#3157,#3158,#3159,#3160));
#997=EDGE_LOOP('',(#3161,#3162,#3163,#3164));
#998=EDGE_LOOP('',(#3165,#3166,#3167,#3168));
#999=EDGE_LOOP('',(#3169));
#1000=EDGE_LOOP('',(#3170));
#1001=EDGE_LOOP('',(#3171));
#1002=EDGE_LOOP('',(#3172));
#1003=EDGE_LOOP('',(#3173,#3174,#3175,#3176));
#1004=EDGE_LOOP('',(#3177,#3178,#3179,#3180));
#1005=EDGE_LOOP('',(#3181));
#1006=EDGE_LOOP('',(#3182));
#1007=EDGE_LOOP('',(#3183));
#1008=EDGE_LOOP('',(#3184));
#1009=EDGE_LOOP('',(#3185));
#1010=EDGE_LOOP('',(#3186));
#1011=EDGE_LOOP('',(#3187,#3188,#3189,#3190));
#1012=EDGE_LOOP('',(#3191,#3192,#3193,#3194));
#1013=EDGE_LOOP('',(#3195));
#1014=EDGE_LOOP('',(#3196));
#1015=EDGE_LOOP('',(#3197));
#1016=EDGE_LOOP('',(#3198));
#1017=EDGE_LOOP('',(#3199));
#1018=EDGE_LOOP('',(#3200));
#1019=EDGE_LOOP('',(#3201,#3202,#3203,#3204));
#1020=EDGE_LOOP('',(#3205,#3206,#3207,#3208));
#1021=EDGE_LOOP('',(#3209));
#1022=EDGE_LOOP('',(#3210));
#1023=EDGE_LOOP('',(#3211));
#1024=EDGE_LOOP('',(#3212));
#1025=EDGE_LOOP('',(#3213,#3214));
#1026=EDGE_LOOP('',(#3215,#3216,#3217,#3218,#3219,#3220,#3221,#3222,#3223));
#1027=EDGE_LOOP('',(#3224,#3225));
#1028=EDGE_LOOP('',(#3226,#3227,#3228,#3229));
#1029=EDGE_LOOP('',(#3230,#3231,#3232,#3233,#3234));
#1030=EDGE_LOOP('',(#3235,#3236,#3237,#3238));
#1031=EDGE_LOOP('',(#3239,#3240));
#1032=EDGE_LOOP('',(#3241));
#1033=EDGE_LOOP('',(#3242));
#1034=EDGE_LOOP('',(#3243));
#1035=EDGE_LOOP('',(#3244));
#1036=EDGE_LOOP('',(#3245,#3246,#3247,#3248));
#1037=EDGE_LOOP('',(#3249,#3250,#3251,#3252));
#1038=EDGE_LOOP('',(#3253,#3254,#3255,#3256));
#1039=EDGE_LOOP('',(#3257));
#1040=EDGE_LOOP('',(#3258));
#1041=EDGE_LOOP('',(#3259,#3260,#3261,#3262));
#1042=EDGE_LOOP('',(#3263,#3264,#3265,#3266));
#1043=EDGE_LOOP('',(#3267));
#1044=EDGE_LOOP('',(#3268));
#1045=EDGE_LOOP('',(#3269));
#1046=EDGE_LOOP('',(#3270));
#1047=EDGE_LOOP('',(#3271));
#1048=EDGE_LOOP('',(#3272));
#1049=EDGE_LOOP('',(#3273));
#1050=EDGE_LOOP('',(#3274));
#1051=EDGE_LOOP('',(#3275,#3276,#3277,#3278));
#1052=EDGE_LOOP('',(#3279));
#1053=EDGE_LOOP('',(#3280));
#1054=EDGE_LOOP('',(#3281,#3282,#3283,#3284));
#1055=EDGE_LOOP('',(#3285,#3286,#3287,#3288));
#1056=EDGE_LOOP('',(#3289));
#1057=EDGE_LOOP('',(#3290));
#1058=EDGE_LOOP('',(#3291));
#1059=EDGE_LOOP('',(#3292));
#1060=EDGE_LOOP('',(#3293,#3294,#3295,#3296));
#1061=EDGE_LOOP('',(#3297));
#1062=EDGE_LOOP('',(#3298));
#1063=EDGE_LOOP('',(#3299,#3300,#3301,#3302));
#1064=EDGE_LOOP('',(#3303,#3304,#3305,#3306));
#1065=EDGE_LOOP('',(#3307));
#1066=EDGE_LOOP('',(#3308));
#1067=EDGE_LOOP('',(#3309));
#1068=EDGE_LOOP('',(#3310));
#1069=EDGE_LOOP('',(#3311,#3312,#3313,#3314));
#1070=EDGE_LOOP('',(#3315,#3316,#3317,#3318));
#1071=EDGE_LOOP('',(#3319,#3320,#3321,#3322));
#1072=EDGE_LOOP('',(#3323,#3324,#3325,#3326));
#1073=EDGE_LOOP('',(#3327,#3328,#3329,#3330));
#1074=EDGE_LOOP('',(#3331,#3332,#3333,#3334));
#1075=EDGE_LOOP('',(#3335,#3336,#3337,#3338,#3339,#3340));
#1076=EDGE_LOOP('',(#3341,#3342,#3343,#3344,#3345,#3346));
#1077=EDGE_LOOP('',(#3347));
#1078=EDGE_LOOP('',(#3348));
#1079=EDGE_LOOP('',(#3349,#3350,#3351,#3352));
#1080=EDGE_LOOP('',(#3353,#3354,#3355,#3356));
#1081=EDGE_LOOP('',(#3357,#3358,#3359,#3360));
#1082=EDGE_LOOP('',(#3361));
#1083=EDGE_LOOP('',(#3362));
#1084=EDGE_LOOP('',(#3363,#3364,#3365,#3366));
#1085=EDGE_LOOP('',(#3367,#3368,#3369,#3370));
#1086=EDGE_LOOP('',(#3371,#3372,#3373,#3374,#3375,#3376));
#1087=EDGE_LOOP('',(#3377,#3378,#3379,#3380,#3381));
#1088=EDGE_LOOP('',(#3382,#3383,#3384,#3385));
#1089=EDGE_LOOP('',(#3386,#3387,#3388,#3389));
#1090=EDGE_LOOP('',(#3390));
#1091=EDGE_LOOP('',(#3391));
#1092=EDGE_LOOP('',(#3392,#3393,#3394,#3395,#3396));
#1093=EDGE_LOOP('',(#3397));
#1094=EDGE_LOOP('',(#3398));
#1095=EDGE_LOOP('',(#3399,#3400,#3401,#3402));
#1096=EDGE_LOOP('',(#3403,#3404,#3405,#3406,#3407,#3408));
#1097=EDGE_LOOP('',(#3409,#3410,#3411,#3412,#3413));
#1098=EDGE_LOOP('',(#3414));
#1099=EDGE_LOOP('',(#3415));
#1100=EDGE_LOOP('',(#3416,#3417,#3418,#3419));
#1101=EDGE_LOOP('',(#3420,#3421,#3422,#3423));
#1102=EDGE_LOOP('',(#3424,#3425,#3426,#3427));
#1103=EDGE_LOOP('',(#3428));
#1104=EDGE_LOOP('',(#3429));
#1105=EDGE_LOOP('',(#3430,#3431,#3432,#3433,#3434));
#1106=EDGE_LOOP('',(#3435,#3436));
#1107=EDGE_LOOP('',(#3437,#3438));
#1108=EDGE_LOOP('',(#3439,#3440));
#1109=EDGE_LOOP('',(#3441,#3442));
#1110=EDGE_LOOP('',(#3443,#3444));
#1111=EDGE_LOOP('',(#3445,#3446));
#1112=EDGE_LOOP('',(#3447,#3448));
#1113=EDGE_LOOP('',(#3449,#3450));
#1114=EDGE_LOOP('',(#3451,#3452));
#1115=EDGE_LOOP('',(#3453,#3454,#3455,#3456));
#1116=EDGE_LOOP('',(#3457,#3458,#3459,#3460,#3461,#3462,#3463,#3464,#3465,
#3466,#3467,#3468,#3469,#3470,#3471,#3472,#3473,#3474,#3475,#3476,#3477,
#3478));
#1117=EDGE_LOOP('',(#3479,#3480,#3481,#3482));
#1118=EDGE_LOOP('',(#3483,#3484,#3485,#3486));
#1119=EDGE_LOOP('',(#3487,#3488,#3489,#3490));
#1120=EDGE_LOOP('',(#3491,#3492,#3493,#3494));
#1121=EDGE_LOOP('',(#3495,#3496,#3497,#3498));
#1122=EDGE_LOOP('',(#3499,#3500,#3501,#3502));
#1123=EDGE_LOOP('',(#3503,#3504,#3505,#3506,#3507,#3508));
#1124=EDGE_LOOP('',(#3509,#3510,#3511,#3512));
#1125=EDGE_LOOP('',(#3513,#3514,#3515,#3516));
#1126=EDGE_LOOP('',(#3517,#3518,#3519,#3520));
#1127=EDGE_LOOP('',(#3521,#3522,#3523,#3524));
#1128=EDGE_LOOP('',(#3525,#3526,#3527,#3528));
#1129=EDGE_LOOP('',(#3529,#3530,#3531,#3532));
#1130=EDGE_LOOP('',(#3533,#3534,#3535,#3536));
#1131=EDGE_LOOP('',(#3537,#3538,#3539,#3540,#3541,#3542,#3543,#3544,#3545,
#3546,#3547,#3548,#3549,#3550,#3551,#3552,#3553,#3554,#3555,#3556,#3557,
#3558));
#1132=EDGE_LOOP('',(#3559,#3560,#3561,#3562));
#1133=EDGE_LOOP('',(#3563,#3564,#3565,#3566));
#1134=EDGE_LOOP('',(#3567));
#1135=EDGE_LOOP('',(#3568));
#1136=EDGE_LOOP('',(#3569,#3570,#3571,#3572));
#1137=EDGE_LOOP('',(#3573));
#1138=EDGE_LOOP('',(#3574));
#1139=EDGE_LOOP('',(#3575,#3576,#3577,#3578));
#1140=EDGE_LOOP('',(#3579));
#1141=EDGE_LOOP('',(#3580));
#1142=EDGE_LOOP('',(#3581,#3582,#3583,#3584));
#1143=EDGE_LOOP('',(#3585));
#1144=EDGE_LOOP('',(#3586));
#1145=EDGE_LOOP('',(#3587,#3588,#3589,#3590));
#1146=EDGE_LOOP('',(#3591));
#1147=EDGE_LOOP('',(#3592));
#1148=EDGE_LOOP('',(#3593,#3594,#3595,#3596));
#1149=EDGE_LOOP('',(#3597));
#1150=EDGE_LOOP('',(#3598,#3599,#3600,#3601));
#1151=EDGE_LOOP('',(#3602,#3603,#3604,#3605));
#1152=EDGE_LOOP('',(#3606,#3607,#3608,#3609));
#1153=EDGE_LOOP('',(#3610,#3611,#3612,#3613));
#1154=EDGE_LOOP('',(#3614,#3615,#3616,#3617));
#1155=EDGE_LOOP('',(#3618,#3619,#3620,#3621));
#1156=EDGE_LOOP('',(#3622,#3623,#3624,#3625,#3626,#3627));
#1157=EDGE_LOOP('',(#3628));
#1158=EDGE_LOOP('',(#3629,#3630,#3631,#3632,#3633,#3634));
#1159=EDGE_LOOP('',(#3635,#3636,#3637,#3638));
#1160=EDGE_LOOP('',(#3639,#3640,#3641,#3642));
#1161=EDGE_LOOP('',(#3643,#3644,#3645,#3646));
#1162=EDGE_LOOP('',(#3647));
#1163=EDGE_LOOP('',(#3648,#3649,#3650,#3651));
#1164=EDGE_LOOP('',(#3652));
#1165=EDGE_LOOP('',(#3653,#3654,#3655,#3656));
#1166=EDGE_LOOP('',(#3657));
#1167=EDGE_LOOP('',(#3658,#3659,#3660,#3661));
#1168=EDGE_LOOP('',(#3662));
#1169=EDGE_LOOP('',(#3663,#3664,#3665,#3666));
#1170=EDGE_LOOP('',(#3667));
#1171=EDGE_LOOP('',(#3668,#3669,#3670,#3671));
#1172=EDGE_LOOP('',(#3672));
#1173=EDGE_LOOP('',(#3673,#3674,#3675,#3676));
#1174=EDGE_LOOP('',(#3677));
#1175=EDGE_LOOP('',(#3678,#3679,#3680,#3681));
#1176=EDGE_LOOP('',(#3682));
#1177=EDGE_LOOP('',(#3683,#3684,#3685,#3686));
#1178=EDGE_LOOP('',(#3687));
#1179=EDGE_LOOP('',(#3688,#3689,#3690,#3691));
#1180=EDGE_LOOP('',(#3692));
#1181=EDGE_LOOP('',(#3693,#3694,#3695,#3696));
#1182=EDGE_LOOP('',(#3697));
#1183=EDGE_LOOP('',(#3698,#3699,#3700,#3701));
#1184=EDGE_LOOP('',(#3702));
#1185=EDGE_LOOP('',(#3703,#3704,#3705,#3706));
#1186=EDGE_LOOP('',(#3707));
#1187=EDGE_LOOP('',(#3708,#3709,#3710,#3711));
#1188=EDGE_LOOP('',(#3712));
#1189=EDGE_LOOP('',(#3713,#3714,#3715,#3716));
#1190=EDGE_LOOP('',(#3717));
#1191=EDGE_LOOP('',(#3718,#3719,#3720,#3721));
#1192=EDGE_LOOP('',(#3722));
#1193=EDGE_LOOP('',(#3723,#3724,#3725,#3726));
#1194=EDGE_LOOP('',(#3727));
#1195=EDGE_LOOP('',(#3728,#3729,#3730,#3731));
#1196=EDGE_LOOP('',(#3732));
#1197=EDGE_LOOP('',(#3733,#3734,#3735,#3736));
#1198=EDGE_LOOP('',(#3737));
#1199=EDGE_LOOP('',(#3738,#3739,#3740,#3741));
#1200=EDGE_LOOP('',(#3742));
#1201=EDGE_LOOP('',(#3743,#3744,#3745,#3746));
#1202=EDGE_LOOP('',(#3747,#3748,#3749,#3750));
#1203=EDGE_LOOP('',(#3751,#3752,#3753,#3754));
#1204=EDGE_LOOP('',(#3755,#3756,#3757,#3758));
#1205=EDGE_LOOP('',(#3759,#3760,#3761,#3762));
#1206=EDGE_LOOP('',(#3763,#3764,#3765,#3766));
#1207=EDGE_LOOP('',(#3767,#3768,#3769,#3770));
#1208=EDGE_LOOP('',(#3771,#3772,#3773,#3774));
#1209=EDGE_LOOP('',(#3775));
#1210=EDGE_LOOP('',(#3776));
#1211=EDGE_LOOP('',(#3777,#3778,#3779,#3780));
#1212=EDGE_LOOP('',(#3781));
#1213=EDGE_LOOP('',(#3782));
#1214=EDGE_LOOP('',(#3783));
#1215=EDGE_LOOP('',(#3784));
#1216=EDGE_LOOP('',(#3785));
#1217=EDGE_LOOP('',(#3786));
#1218=EDGE_LOOP('',(#3787));
#1219=EDGE_LOOP('',(#3788));
#1220=EDGE_LOOP('',(#3789));
#1221=EDGE_LOOP('',(#3790));
#1222=EDGE_LOOP('',(#3791));
#1223=EDGE_LOOP('',(#3792));
#1224=EDGE_LOOP('',(#3793));
#1225=EDGE_LOOP('',(#3794));
#1226=EDGE_LOOP('',(#3795));
#1227=EDGE_LOOP('',(#3796));
#1228=EDGE_LOOP('',(#3797));
#1229=EDGE_LOOP('',(#3798));
#1230=EDGE_LOOP('',(#3799));
#1231=EDGE_LOOP('',(#3800));
#1232=EDGE_LOOP('',(#3801));
#1233=EDGE_LOOP('',(#3802));
#1234=EDGE_LOOP('',(#3803));
#1235=EDGE_LOOP('',(#3804));
#1236=EDGE_LOOP('',(#3805));
#1237=EDGE_LOOP('',(#3806));
#1238=EDGE_LOOP('',(#3807));
#1239=EDGE_LOOP('',(#3808));
#1240=EDGE_LOOP('',(#3809,#3810,#3811,#3812));
#1241=EDGE_LOOP('',(#3813,#3814,#3815,#3816));
#1242=EDGE_LOOP('',(#3817));
#1243=EDGE_LOOP('',(#3818));
#1244=EDGE_LOOP('',(#3819));
#1245=EDGE_LOOP('',(#3820));
#1246=EDGE_LOOP('',(#3821));
#1247=EDGE_LOOP('',(#3822));
#1248=EDGE_LOOP('',(#3823));
#1249=EDGE_LOOP('',(#3824));
#1250=EDGE_LOOP('',(#3825));
#1251=EDGE_LOOP('',(#3826));
#1252=EDGE_LOOP('',(#3827,#3828,#3829,#3830));
#1253=EDGE_LOOP('',(#3831,#3832,#3833,#3834));
#1254=EDGE_LOOP('',(#3835));
#1255=EDGE_LOOP('',(#3836));
#1256=EDGE_LOOP('',(#3837));
#1257=EDGE_LOOP('',(#3838));
#1258=EDGE_LOOP('',(#3839));
#1259=EDGE_LOOP('',(#3840));
#1260=EDGE_LOOP('',(#3841,#3842,#3843,#3844));
#1261=EDGE_LOOP('',(#3845,#3846,#3847,#3848));
#1262=EDGE_LOOP('',(#3849));
#1263=EDGE_LOOP('',(#3850));
#1264=EDGE_LOOP('',(#3851));
#1265=EDGE_LOOP('',(#3852));
#1266=EDGE_LOOP('',(#3853,#3854,#3855,#3856));
#1267=EDGE_LOOP('',(#3857,#3858,#3859,#3860));
#1268=EDGE_LOOP('',(#3861,#3862,#3863,#3864));
#1269=EDGE_LOOP('',(#3865,#3866,#3867,#3868));
#1270=EDGE_LOOP('',(#3869,#3870,#3871,#3872));
#1271=EDGE_LOOP('',(#3873));
#1272=EDGE_LOOP('',(#3874));
#1273=EDGE_LOOP('',(#3875,#3876,#3877,#3878));
#1274=EDGE_LOOP('',(#3879,#3880,#3881,#3882));
#1275=EDGE_LOOP('',(#3883));
#1276=EDGE_LOOP('',(#3884));
#1277=EDGE_LOOP('',(#3885));
#1278=EDGE_LOOP('',(#3886));
#1279=EDGE_LOOP('',(#3887));
#1280=EDGE_LOOP('',(#3888));
#1281=EDGE_LOOP('',(#3889));
#1282=EDGE_LOOP('',(#3890));
#1283=EDGE_LOOP('',(#3891));
#1284=EDGE_LOOP('',(#3892));
#1285=EDGE_LOOP('',(#3893));
#1286=EDGE_LOOP('',(#3894));
#1287=EDGE_LOOP('',(#3895,#3896,#3897,#3898));
#1288=EDGE_LOOP('',(#3899,#3900,#3901,#3902));
#1289=EDGE_LOOP('',(#3903,#3904,#3905,#3906));
#1290=EDGE_LOOP('',(#3907,#3908,#3909,#3910));
#1291=EDGE_LOOP('',(#3911,#3912,#3913,#3914));
#1292=EDGE_LOOP('',(#3915,#3916,#3917,#3918));
#1293=EDGE_LOOP('',(#3919,#3920,#3921,#3922));
#1294=EDGE_LOOP('',(#3923,#3924,#3925,#3926));
#1295=EDGE_LOOP('',(#3927,#3928,#3929,#3930));
#1296=EDGE_LOOP('',(#3931,#3932,#3933,#3934));
#1297=EDGE_LOOP('',(#3935,#3936,#3937,#3938));
#1298=EDGE_LOOP('',(#3939,#3940,#3941,#3942));
#1299=EDGE_LOOP('',(#3943,#3944,#3945,#3946));
#1300=EDGE_LOOP('',(#3947,#3948,#3949,#3950));
#1301=EDGE_LOOP('',(#3951,#3952,#3953,#3954));
#1302=EDGE_LOOP('',(#3955,#3956,#3957,#3958));
#1303=EDGE_LOOP('',(#3959,#3960,#3961,#3962));
#1304=EDGE_LOOP('',(#3963,#3964,#3965,#3966));
#1305=EDGE_LOOP('',(#3967));
#1306=EDGE_LOOP('',(#3968));
#1307=EDGE_LOOP('',(#3969));
#1308=EDGE_LOOP('',(#3970));
#1309=EDGE_LOOP('',(#3971));
#1310=EDGE_LOOP('',(#3972));
#1311=EDGE_LOOP('',(#3973));
#1312=EDGE_LOOP('',(#3974));
#1313=EDGE_LOOP('',(#3975));
#1314=EDGE_LOOP('',(#3976));
#1315=EDGE_LOOP('',(#3977));
#1316=EDGE_LOOP('',(#3978));
#1317=EDGE_LOOP('',(#3979));
#1318=EDGE_LOOP('',(#3980));
#1319=EDGE_LOOP('',(#3981));
#1320=EDGE_LOOP('',(#3982));
#1321=EDGE_LOOP('',(#3983));
#1322=EDGE_LOOP('',(#3984));
#1323=EDGE_LOOP('',(#3985));
#1324=EDGE_LOOP('',(#3986));
#1325=EDGE_LOOP('',(#3987));
#1326=EDGE_LOOP('',(#3988));
#1327=EDGE_LOOP('',(#3989));
#1328=EDGE_LOOP('',(#3990));
#1329=EDGE_LOOP('',(#3991));
#1330=EDGE_LOOP('',(#3992));
#1331=EDGE_LOOP('',(#3993));
#1332=EDGE_LOOP('',(#3994));
#1333=EDGE_LOOP('',(#3995));
#1334=EDGE_LOOP('',(#3996));
#1335=EDGE_LOOP('',(#3997));
#1336=EDGE_LOOP('',(#3998));
#1337=EDGE_LOOP('',(#3999));
#1338=EDGE_LOOP('',(#4000));
#1339=EDGE_LOOP('',(#4001));
#1340=EDGE_LOOP('',(#4002));
#1341=EDGE_LOOP('',(#4003));
#1342=EDGE_LOOP('',(#4004,#4005,#4006,#4007));
#1343=EDGE_LOOP('',(#4008,#4009,#4010,#4011));
#1344=EDGE_LOOP('',(#4012,#4013,#4014,#4015));
#1345=EDGE_LOOP('',(#4016));
#1346=EDGE_LOOP('',(#4017));
#1347=EDGE_LOOP('',(#4018,#4019,#4020,#4021));
#1348=EDGE_LOOP('',(#4022,#4023,#4024,#4025));
#1349=EDGE_LOOP('',(#4026,#4027,#4028,#4029));
#1350=EDGE_LOOP('',(#4030));
#1351=EDGE_LOOP('',(#4031,#4032,#4033,#4034));
#1352=EDGE_LOOP('',(#4035,#4036,#4037,#4038));
#1353=EDGE_LOOP('',(#4039,#4040,#4041,#4042));
#1354=EDGE_LOOP('',(#4043,#4044,#4045,#4046));
#1355=EDGE_LOOP('',(#4047,#4048,#4049,#4050));
#1356=EDGE_LOOP('',(#4051,#4052,#4053,#4054));
#1357=EDGE_LOOP('',(#4055,#4056,#4057,#4058,#4059,#4060));
#1358=EDGE_LOOP('',(#4061,#4062,#4063,#4064,#4065,#4066));
#1359=EDGE_LOOP('',(#4067));
#1360=EDGE_LOOP('',(#4068));
#1361=EDGE_LOOP('',(#4069));
#1362=EDGE_LOOP('',(#4070));
#1363=EDGE_LOOP('',(#4071));
#1364=EDGE_LOOP('',(#4072,#4073,#4074,#4075));
#1365=EDGE_LOOP('',(#4076,#4077,#4078,#4079));
#1366=EDGE_LOOP('',(#4080,#4081,#4082,#4083));
#1367=EDGE_LOOP('',(#4084));
#1368=EDGE_LOOP('',(#4085,#4086));
#1369=EDGE_LOOP('',(#4087,#4088,#4089,#4090,#4091,#4092,#4093,#4094,#4095));
#1370=EDGE_LOOP('',(#4096,#4097));
#1371=EDGE_LOOP('',(#4098,#4099,#4100,#4101));
#1372=EDGE_LOOP('',(#4102,#4103,#4104,#4105,#4106));
#1373=EDGE_LOOP('',(#4107,#4108,#4109,#4110));
#1374=EDGE_LOOP('',(#4111,#4112));
#1375=EDGE_LOOP('',(#4113));
#1376=EDGE_LOOP('',(#4114));
#1377=EDGE_LOOP('',(#4115));
#1378=EDGE_LOOP('',(#4116));
#1379=EDGE_LOOP('',(#4117,#4118,#4119,#4120));
#1380=EDGE_LOOP('',(#4121,#4122,#4123,#4124));
#1381=EDGE_LOOP('',(#4125,#4126,#4127,#4128));
#1382=EDGE_LOOP('',(#4129,#4130,#4131,#4132));
#1383=EDGE_LOOP('',(#4133,#4134,#4135,#4136));
#1384=EDGE_LOOP('',(#4137,#4138,#4139,#4140));
#1385=EDGE_LOOP('',(#4141,#4142,#4143,#4144,#4145,#4146));
#1386=EDGE_LOOP('',(#4147));
#1387=EDGE_LOOP('',(#4148,#4149,#4150,#4151,#4152,#4153));
#1388=EDGE_LOOP('',(#4154,#4155,#4156,#4157));
#1389=EDGE_LOOP('',(#4158,#4159,#4160,#4161));
#1390=EDGE_LOOP('',(#4162,#4163,#4164,#4165));
#1391=EDGE_LOOP('',(#4166));
#1392=LINE('',#7132,#1612);
#1393=LINE('',#7138,#1613);
#1394=LINE('',#7144,#1614);
#1395=LINE('',#7150,#1615);
#1396=LINE('',#7156,#1616);
#1397=LINE('',#7162,#1617);
#1398=LINE('',#7168,#1618);
#1399=LINE('',#7173,#1619);
#1400=LINE('',#7175,#1620);
#1401=LINE('',#7177,#1621);
#1402=LINE('',#7178,#1622);
#1403=LINE('',#7181,#1623);
#1404=LINE('',#7183,#1624);
#1405=LINE('',#7184,#1625);
#1406=LINE('',#7187,#1626);
#1407=LINE('',#7189,#1627);
#1408=LINE('',#7190,#1628);
#1409=LINE('',#7192,#1629);
#1410=LINE('',#7193,#1630);
#1411=LINE('',#7201,#1631);
#1412=LINE('',#7210,#1632);
#1413=LINE('',#7219,#1633);
#1414=LINE('',#7228,#1634);
#1415=LINE('',#7237,#1635);
#1416=LINE('',#7243,#1636);
#1417=LINE('',#7249,#1637);
#1418=LINE('',#7255,#1638);
#1419=LINE('',#7268,#1639);
#1420=LINE('',#7271,#1640);
#1421=LINE('',#7278,#1641);
#1422=LINE('',#7283,#1642);
#1423=LINE('',#7291,#1643);
#1424=LINE('',#7297,#1644);
#1425=LINE('',#7305,#1645);
#1426=LINE('',#7335,#1646);
#1427=LINE('',#7382,#1647);
#1428=LINE('',#7387,#1648);
#1429=LINE('',#7393,#1649);
#1430=LINE('',#7402,#1650);
#1431=LINE('',#7408,#1651);
#1432=LINE('',#7414,#1652);
#1433=LINE('',#7421,#1653);
#1434=LINE('',#7427,#1654);
#1435=LINE('',#7436,#1655);
#1436=LINE('',#7443,#1656);
#1437=LINE('',#7449,#1657);
#1438=LINE('',#8521,#1658);
#1439=LINE('',#8527,#1659);
#1440=LINE('',#8535,#1660);
#1441=LINE('',#8537,#1661);
#1442=LINE('',#8539,#1662);
#1443=LINE('',#8540,#1663);
#1444=LINE('',#8543,#1664);
#1445=LINE('',#8545,#1665);
#1446=LINE('',#8546,#1666);
#1447=LINE('',#8549,#1667);
#1448=LINE('',#8551,#1668);
#1449=LINE('',#8552,#1669);
#1450=LINE('',#8555,#1670);
#1451=LINE('',#8557,#1671);
#1452=LINE('',#8558,#1672);
#1453=LINE('',#8561,#1673);
#1454=LINE('',#8563,#1674);
#1455=LINE('',#8564,#1675);
#1456=LINE('',#8566,#1676);
#1457=LINE('',#8567,#1677);
#1458=LINE('',#8579,#1678);
#1459=LINE('',#8583,#1679);
#1460=LINE('',#8587,#1680);
#1461=LINE('',#8594,#1681);
#1462=LINE('',#8596,#1682);
#1463=LINE('',#8611,#1683);
#1464=LINE('',#8617,#1684);
#1465=LINE('',#8621,#1685);
#1466=LINE('',#8627,#1686);
#1467=LINE('',#8632,#1687);
#1468=LINE('',#8647,#1688);
#1469=LINE('',#8656,#1689);
#1470=LINE('',#8660,#1690);
#1471=LINE('',#8664,#1691);
#1472=LINE('',#8667,#1692);
#1473=LINE('',#8836,#1693);
#1474=LINE('',#9172,#1694);
#1475=LINE('',#9214,#1695);
#1476=LINE('',#9219,#1696);
#1477=LINE('',#9228,#1697);
#1478=LINE('',#9233,#1698);
#1479=LINE('',#9246,#1699);
#1480=LINE('',#9248,#1700);
#1481=LINE('',#9250,#1701);
#1482=LINE('',#9251,#1702);
#1483=LINE('',#9254,#1703);
#1484=LINE('',#9256,#1704);
#1485=LINE('',#9257,#1705);
#1486=LINE('',#9260,#1706);
#1487=LINE('',#9262,#1707);
#1488=LINE('',#9263,#1708);
#1489=LINE('',#9266,#1709);
#1490=LINE('',#9268,#1710);
#1491=LINE('',#9269,#1711);
#1492=LINE('',#9272,#1712);
#1493=LINE('',#9274,#1713);
#1494=LINE('',#9275,#1714);
#1495=LINE('',#9277,#1715);
#1496=LINE('',#9278,#1716);
#1497=LINE('',#9286,#1717);
#1498=LINE('',#9288,#1718);
#1499=LINE('',#9295,#1719);
#1500=LINE('',#9302,#1720);
#1501=LINE('',#9309,#1721);
#1502=LINE('',#9316,#1722);
#1503=LINE('',#9323,#1723);
#1504=LINE('',#9330,#1724);
#1505=LINE('',#9337,#1725);
#1506=LINE('',#9344,#1726);
#1507=LINE('',#9351,#1727);
#1508=LINE('',#9358,#1728);
#1509=LINE('',#9365,#1729);
#1510=LINE('',#9372,#1730);
#1511=LINE('',#9379,#1731);
#1512=LINE('',#9386,#1732);
#1513=LINE('',#9393,#1733);
#1514=LINE('',#9400,#1734);
#1515=LINE('',#9407,#1735);
#1516=LINE('',#9414,#1736);
#1517=LINE('',#9421,#1737);
#1518=LINE('',#9428,#1738);
#1519=LINE('',#9435,#1739);
#1520=LINE('',#9441,#1740);
#1521=LINE('',#9447,#1741);
#1522=LINE('',#9453,#1742);
#1523=LINE('',#9459,#1743);
#1524=LINE('',#9465,#1744);
#1525=LINE('',#9471,#1745);
#1526=LINE('',#9477,#1746);
#1527=LINE('',#9486,#1747);
#1528=LINE('',#9499,#1748);
#1529=LINE('',#9503,#1749);
#1530=LINE('',#9507,#1750);
#1531=LINE('',#9511,#1751);
#1532=LINE('',#9519,#1752);
#1533=LINE('',#9525,#1753);
#1534=LINE('',#9534,#1754);
#1535=LINE('',#9540,#1755);
#1536=LINE('',#9546,#1756);
#1537=LINE('',#9552,#1757);
#1538=LINE('',#9558,#1758);
#1539=LINE('',#9565,#1759);
#1540=LINE('',#9571,#1760);
#1541=LINE('',#9580,#1761);
#1542=LINE('',#9586,#1762);
#1543=LINE('',#9592,#1763);
#1544=LINE('',#9598,#1764);
#1545=LINE('',#9604,#1765);
#1546=LINE('',#9610,#1766);
#1547=LINE('',#9616,#1767);
#1548=LINE('',#9622,#1768);
#1549=LINE('',#9628,#1769);
#1550=LINE('',#9634,#1770);
#1551=LINE('',#9640,#1771);
#1552=LINE('',#9646,#1772);
#1553=LINE('',#9652,#1773);
#1554=LINE('',#9658,#1774);
#1555=LINE('',#9664,#1775);
#1556=LINE('',#9670,#1776);
#1557=LINE('',#9676,#1777);
#1558=LINE('',#9682,#1778);
#1559=LINE('',#9693,#1779);
#1560=LINE('',#9697,#1780);
#1561=LINE('',#9701,#1781);
#1562=LINE('',#9708,#1782);
#1563=LINE('',#9712,#1783);
#1564=LINE('',#9716,#1784);
#1565=LINE('',#9721,#1785);
#1566=LINE('',#9723,#1786);
#1567=LINE('',#9725,#1787);
#1568=LINE('',#9726,#1788);
#1569=LINE('',#9729,#1789);
#1570=LINE('',#9731,#1790);
#1571=LINE('',#9732,#1791);
#1572=LINE('',#9735,#1792);
#1573=LINE('',#9737,#1793);
#1574=LINE('',#9738,#1794);
#1575=LINE('',#9741,#1795);
#1576=LINE('',#9743,#1796);
#1577=LINE('',#9744,#1797);
#1578=LINE('',#9747,#1798);
#1579=LINE('',#9749,#1799);
#1580=LINE('',#9750,#1800);
#1581=LINE('',#9752,#1801);
#1582=LINE('',#9753,#1802);
#1583=LINE('',#9807,#1803);
#1584=LINE('',#9809,#1804);
#1585=LINE('',#9813,#1805);
#1586=LINE('',#9819,#1806);
#1587=LINE('',#9837,#1807);
#1588=LINE('',#9880,#1808);
#1589=LINE('',#9885,#1809);
#1590=LINE('',#9891,#1810);
#1591=LINE('',#9899,#1811);
#1592=LINE('',#9901,#1812);
#1593=LINE('',#9903,#1813);
#1594=LINE('',#9904,#1814);
#1595=LINE('',#9907,#1815);
#1596=LINE('',#9909,#1816);
#1597=LINE('',#9910,#1817);
#1598=LINE('',#9913,#1818);
#1599=LINE('',#9915,#1819);
#1600=LINE('',#9916,#1820);
#1601=LINE('',#9919,#1821);
#1602=LINE('',#9921,#1822);
#1603=LINE('',#9922,#1823);
#1604=LINE('',#9925,#1824);
#1605=LINE('',#9927,#1825);
#1606=LINE('',#9928,#1826);
#1607=LINE('',#9930,#1827);
#1608=LINE('',#9931,#1828);
#1609=LINE('',#9939,#1829);
#1610=LINE('',#9943,#1830);
#1611=LINE('',#9947,#1831);
#1612=VECTOR('',#5583,0.165);
#1613=VECTOR('',#5590,0.165);
#1614=VECTOR('',#5597,0.31);
#1615=VECTOR('',#5604,0.25);
#1616=VECTOR('',#5611,0.25);
#1617=VECTOR('',#5618,0.25);
#1618=VECTOR('',#5625,0.25);
#1619=VECTOR('',#5630,1.);
#1620=VECTOR('',#5631,1.);
#1621=VECTOR('',#5632,1.);
#1622=VECTOR('',#5633,1.);
#1623=VECTOR('',#5636,1.);
#1624=VECTOR('',#5637,1.);
#1625=VECTOR('',#5638,1.);
#1626=VECTOR('',#5641,1.);
#1627=VECTOR('',#5642,1.);
#1628=VECTOR('',#5643,1.);
#1629=VECTOR('',#5646,1.);
#1630=VECTOR('',#5647,1.);
#1631=VECTOR('',#5658,1.);
#1632=VECTOR('',#5671,1.);
#1633=VECTOR('',#5684,1.);
#1634=VECTOR('',#5697,1.);
#1635=VECTOR('',#5710,0.33);
#1636=VECTOR('',#5717,0.33);
#1637=VECTOR('',#5724,0.33);
#1638=VECTOR('',#5731,0.33);
#1639=VECTOR('',#5748,1.6);
#1640=VECTOR('',#5751,1.25);
#1641=VECTOR('',#5760,3.5);
#1642=VECTOR('',#5767,1.25);
#1643=VECTOR('',#5778,1.255);
#1644=VECTOR('',#5785,1.7);
#1645=VECTOR('',#5796,1.);
#1646=VECTOR('',#5803,0.21);
#1647=VECTOR('',#5806,1.);
#1648=VECTOR('',#5811,1.255);
#1649=VECTOR('',#5818,1.8);
#1650=VECTOR('',#5831,0.225);
#1651=VECTOR('',#5838,0.225);
#1652=VECTOR('',#5845,0.999999999999999);
#1653=VECTOR('',#5854,0.31);
#1654=VECTOR('',#5861,2.);
#1655=VECTOR('',#5874,0.31);
#1656=VECTOR('',#5883,0.6);
#1657=VECTOR('',#5890,0.999999999999999);
#1658=VECTOR('',#5913,0.32);
#1659=VECTOR('',#5920,0.6);
#1660=VECTOR('',#5931,1.);
#1661=VECTOR('',#5932,1.);
#1662=VECTOR('',#5933,1.);
#1663=VECTOR('',#5934,1.);
#1664=VECTOR('',#5937,1.);
#1665=VECTOR('',#5938,1.);
#1666=VECTOR('',#5939,1.);
#1667=VECTOR('',#5942,1.);
#1668=VECTOR('',#5943,1.);
#1669=VECTOR('',#5944,1.);
#1670=VECTOR('',#5947,1.);
#1671=VECTOR('',#5948,1.);
#1672=VECTOR('',#5949,1.);
#1673=VECTOR('',#5952,1.);
#1674=VECTOR('',#5953,1.);
#1675=VECTOR('',#5954,1.);
#1676=VECTOR('',#5957,1.);
#1677=VECTOR('',#5958,1.);
#1678=VECTOR('',#5975,0.475);
#1679=VECTOR('',#5980,0.5);
#1680=VECTOR('',#5985,0.485);
#1681=VECTOR('',#5994,0.31);
#1682=VECTOR('',#5997,0.3);
#1683=VECTOR('',#6016,1.88531);
#1684=VECTOR('',#6023,1.25);
#1685=VECTOR('',#6028,1.3);
#1686=VECTOR('',#6037,1.88531);
#1687=VECTOR('',#6044,1.3);
#1688=VECTOR('',#6063,1.96469);
#1689=VECTOR('',#6074,2.55);
#1690=VECTOR('',#6079,2.6);
#1691=VECTOR('',#6084,2.55);
#1692=VECTOR('',#6089,1.96469);
#1693=VECTOR('',#6146,1.956752);
#1694=VECTOR('',#6237,1.893248);
#1695=VECTOR('',#6266,1.95469);
#1696=VECTOR('',#6273,1.90031);
#1697=VECTOR('',#6284,1.95469);
#1698=VECTOR('',#6291,1.90031);
#1699=VECTOR('',#6310,1.);
#1700=VECTOR('',#6311,1.);
#1701=VECTOR('',#6312,1.);
#1702=VECTOR('',#6313,1.);
#1703=VECTOR('',#6316,1.);
#1704=VECTOR('',#6317,1.);
#1705=VECTOR('',#6318,1.);
#1706=VECTOR('',#6321,1.);
#1707=VECTOR('',#6322,1.);
#1708=VECTOR('',#6323,1.);
#1709=VECTOR('',#6326,1.);
#1710=VECTOR('',#6327,1.);
#1711=VECTOR('',#6328,1.);
#1712=VECTOR('',#6331,1.);
#1713=VECTOR('',#6332,1.);
#1714=VECTOR('',#6333,1.);
#1715=VECTOR('',#6336,1.);
#1716=VECTOR('',#6337,1.);
#1717=VECTOR('',#6348,0.235);
#1718=VECTOR('',#6351,0.25);
#1719=VECTOR('',#6360,0.165);
#1720=VECTOR('',#6369,0.165);
#1721=VECTOR('',#6378,0.165);
#1722=VECTOR('',#6387,0.165);
#1723=VECTOR('',#6396,0.31);
#1724=VECTOR('',#6405,0.31);
#1725=VECTOR('',#6414,0.31);
#1726=VECTOR('',#6423,0.31);
#1727=VECTOR('',#6432,0.31);
#1728=VECTOR('',#6441,0.31);
#1729=VECTOR('',#6450,0.31);
#1730=VECTOR('',#6459,0.31);
#1731=VECTOR('',#6468,0.31);
#1732=VECTOR('',#6477,0.31);
#1733=VECTOR('',#6486,0.31);
#1734=VECTOR('',#6495,0.31);
#1735=VECTOR('',#6504,0.165);
#1736=VECTOR('',#6513,0.165);
#1737=VECTOR('',#6522,0.165);
#1738=VECTOR('',#6531,0.165);
#1739=VECTOR('',#6540,0.33);
#1740=VECTOR('',#6547,0.33);
#1741=VECTOR('',#6554,0.33);
#1742=VECTOR('',#6561,0.33);
#1743=VECTOR('',#6568,0.33);
#1744=VECTOR('',#6575,0.33);
#1745=VECTOR('',#6582,0.33);
#1746=VECTOR('',#6589,0.33);
#1747=VECTOR('',#6600,1.9);
#1748=VECTOR('',#6617,2.);
#1749=VECTOR('',#6622,10.);
#1750=VECTOR('',#6627,2.6);
#1751=VECTOR('',#6632,4.);
#1752=VECTOR('',#6643,2.);
#1753=VECTOR('',#6650,2.59);
#1754=VECTOR('',#6663,0.225);
#1755=VECTOR('',#6670,0.225);
#1756=VECTOR('',#6677,0.225);
#1757=VECTOR('',#6684,0.225);
#1758=VECTOR('',#6691,2.59);
#1759=VECTOR('',#6700,1.9);
#1760=VECTOR('',#6707,4.);
#1761=VECTOR('',#6720,0.225);
#1762=VECTOR('',#6727,0.225);
#1763=VECTOR('',#6734,0.225);
#1764=VECTOR('',#6741,0.225);
#1765=VECTOR('',#6748,0.31);
#1766=VECTOR('',#6755,0.31);
#1767=VECTOR('',#6762,0.31);
#1768=VECTOR('',#6769,0.31);
#1769=VECTOR('',#6776,0.31);
#1770=VECTOR('',#6783,0.31);
#1771=VECTOR('',#6790,0.31);
#1772=VECTOR('',#6797,0.31);
#1773=VECTOR('',#6804,0.31);
#1774=VECTOR('',#6811,0.31);
#1775=VECTOR('',#6818,0.31);
#1776=VECTOR('',#6825,0.31);
#1777=VECTOR('',#6832,6.5);
#1778=VECTOR('',#6839,8.);
#1779=VECTOR('',#6856,0.325);
#1780=VECTOR('',#6861,0.35);
#1781=VECTOR('',#6866,0.335);
#1782=VECTOR('',#6875,0.21);
#1783=VECTOR('',#6880,0.2);
#1784=VECTOR('',#6885,0.18);
#1785=VECTOR('',#6890,1.);
#1786=VECTOR('',#6891,1.);
#1787=VECTOR('',#6892,1.);
#1788=VECTOR('',#6893,1.);
#1789=VECTOR('',#6896,1.);
#1790=VECTOR('',#6897,1.);
#1791=VECTOR('',#6898,1.);
#1792=VECTOR('',#6901,1.);
#1793=VECTOR('',#6902,1.);
#1794=VECTOR('',#6903,1.);
#1795=VECTOR('',#6906,1.);
#1796=VECTOR('',#6907,1.);
#1797=VECTOR('',#6908,1.);
#1798=VECTOR('',#6911,1.);
#1799=VECTOR('',#6912,1.);
#1800=VECTOR('',#6913,1.);
#1801=VECTOR('',#6916,1.);
#1802=VECTOR('',#6917,1.);
#1803=VECTOR('',#7014,0.5);
#1804=VECTOR('',#7017,0.3);
#1805=VECTOR('',#7022,0.3);
#1806=VECTOR('',#7029,1.);
#1807=VECTOR('',#7036,0.21);
#1808=VECTOR('',#7039,1.);
#1809=VECTOR('',#7044,0.3);
#1810=VECTOR('',#7051,1.2);
#1811=VECTOR('',#7062,1.);
#1812=VECTOR('',#7063,1.);
#1813=VECTOR('',#7064,1.);
#1814=VECTOR('',#7065,1.);
#1815=VECTOR('',#7068,1.);
#1816=VECTOR('',#7069,1.);
#1817=VECTOR('',#7070,1.);
#1818=VECTOR('',#7073,1.);
#1819=VECTOR('',#7074,1.);
#1820=VECTOR('',#7075,1.);
#1821=VECTOR('',#7078,1.);
#1822=VECTOR('',#7079,1.);
#1823=VECTOR('',#7080,1.);
#1824=VECTOR('',#7083,1.);
#1825=VECTOR('',#7084,1.);
#1826=VECTOR('',#7085,1.);
#1827=VECTOR('',#7088,1.);
#1828=VECTOR('',#7089,1.);
#1829=VECTOR('',#7100,0.235);
#1830=VECTOR('',#7105,0.25);
#1831=VECTOR('',#7110,0.2125);
#1832=CIRCLE('',#4911,0.165);
#1833=CIRCLE('',#4912,0.165);
#1834=CIRCLE('',#4914,0.165);
#1835=CIRCLE('',#4915,0.165);
#1836=CIRCLE('',#4917,0.31);
#1837=CIRCLE('',#4918,0.31);
#1838=CIRCLE('',#4920,0.25);
#1839=CIRCLE('',#4921,0.25);
#1840=CIRCLE('',#4923,0.25);
#1841=CIRCLE('',#4924,0.25);
#1842=CIRCLE('',#4926,0.25);
#1843=CIRCLE('',#4927,0.25);
#1844=CIRCLE('',#4929,0.25);
#1845=CIRCLE('',#4930,0.25);
#1846=CIRCLE('',#4939,1.);
#1847=CIRCLE('',#4940,1.);
#1848=CIRCLE('',#4945,1.);
#1849=CIRCLE('',#4946,1.);
#1850=CIRCLE('',#4951,1.);
#1851=CIRCLE('',#4952,1.);
#1852=CIRCLE('',#4957,1.);
#1853=CIRCLE('',#4958,1.);
#1854=CIRCLE('',#4963,0.33);
#1855=CIRCLE('',#4964,0.33);
#1856=CIRCLE('',#4966,0.33);
#1857=CIRCLE('',#4967,0.33);
#1858=CIRCLE('',#4969,0.33);
#1859=CIRCLE('',#4970,0.33);
#1860=CIRCLE('',#4972,0.33);
#1861=CIRCLE('',#4973,0.33);
#1862=CIRCLE('',#4975,1.6);
#1863=CIRCLE('',#4976,1.25);
#1864=CIRCLE('',#4978,1.6);
#1865=CIRCLE('',#4979,1.25);
#1866=CIRCLE('',#4982,1.25);
#1867=CIRCLE('',#4984,3.5);
#1868=CIRCLE('',#4986,3.5);
#1869=CIRCLE('',#4988,1.25);
#1870=CIRCLE('',#4993,1.255);
#1871=CIRCLE('',#4994,1.255);
#1872=CIRCLE('',#4996,1.7);
#1873=CIRCLE('',#4997,1.7);
#1874=CIRCLE('',#5002,0.21);
#1875=CIRCLE('',#5004,0.21);
#1876=CIRCLE('',#5007,1.255);
#1877=CIRCLE('',#5008,1.255);
#1878=CIRCLE('',#5010,1.8);
#1879=CIRCLE('',#5011,1.8);
#1880=CIRCLE('',#5016,0.225);
#1881=CIRCLE('',#5017,0.225);
#1882=CIRCLE('',#5019,0.225);
#1883=CIRCLE('',#5020,0.225);
#1884=CIRCLE('',#5022,0.999999999999999);
#1885=CIRCLE('',#5023,0.999999999999999);
#1886=CIRCLE('',#5025,0.31);
#1887=CIRCLE('',#5027,0.31);
#1888=CIRCLE('',#5029,2.);
#1889=CIRCLE('',#5030,2.);
#1890=CIRCLE('',#5035,0.31);
#1891=CIRCLE('',#5036,0.31);
#1892=CIRCLE('',#5038,0.6);
#1893=CIRCLE('',#5040,0.6);
#1894=CIRCLE('',#5042,0.999999999999999);
#1895=CIRCLE('',#5043,0.999999999999999);
#1896=CIRCLE('',#5047,0.05);
#1897=CIRCLE('',#5048,0.05);
#1898=CIRCLE('',#5053,0.32);
#1899=CIRCLE('',#5054,0.32);
#1900=CIRCLE('',#5056,0.6);
#1901=CIRCLE('',#5057,0.6);
#1902=CIRCLE('',#5070,0.2942);
#1903=CIRCLE('',#5072,0.45);
#1904=CIRCLE('',#5074,0.5);
#1905=CIRCLE('',#5076,0.5);
#1906=CIRCLE('',#5078,0.47);
#1907=CIRCLE('',#5080,0.32);
#1908=CIRCLE('',#5082,0.2942);
#1909=CIRCLE('',#5087,1.88531);
#1910=CIRCLE('',#5088,1.88531);
#1911=CIRCLE('',#5089,0.412776);
#1912=CIRCLE('',#5090,1.88531);
#1913=CIRCLE('',#5091,1.88531);
#1914=CIRCLE('',#5093,1.88531);
#1915=CIRCLE('',#5095,1.25);
#1916=CIRCLE('',#5096,1.25);
#1917=CIRCLE('',#5098,1.35);
#1918=CIRCLE('',#5101,1.88531);
#1919=CIRCLE('',#5103,1.35);
#1920=CIRCLE('',#5107,1.96469);
#1921=CIRCLE('',#5108,1.96469);
#1922=CIRCLE('',#5109,0.412776);
#1923=CIRCLE('',#5110,1.96469);
#1924=CIRCLE('',#5111,1.96469);
#1925=CIRCLE('',#5113,1.96469);
#1926=CIRCLE('',#5115,2.5);
#1927=CIRCLE('',#5116,1.96469);
#1928=CIRCLE('',#5118,2.6);
#1929=CIRCLE('',#5120,2.6);
#1930=CIRCLE('',#5122,2.5);
#1931=CIRCLE('',#5127,0.3969);
#1932=CIRCLE('',#5129,0.3969);
#1933=CIRCLE('',#5131,0.3969);
#1934=CIRCLE('',#5133,0.3969);
#1935=CIRCLE('',#5135,0.3969);
#1936=CIRCLE('',#5137,0.3969);
#1937=CIRCLE('',#5139,0.3969);
#1938=CIRCLE('',#5141,0.3969);
#1939=CIRCLE('',#5143,0.3969);
#1940=CIRCLE('',#5146,0.405071403305639);
#1941=CIRCLE('',#5147,0.405071403305639);
#1942=CIRCLE('',#5149,1.956752);
#1943=CIRCLE('',#5150,1.956752);
#1944=CIRCLE('',#5151,1.956752);
#1945=CIRCLE('',#5152,1.956752);
#1946=CIRCLE('',#5153,1.956752);
#1947=CIRCLE('',#5154,1.956752);
#1948=CIRCLE('',#5155,1.956752);
#1949=CIRCLE('',#5156,1.956752);
#1950=CIRCLE('',#5157,1.956752);
#1951=CIRCLE('',#5158,1.956752);
#1952=CIRCLE('',#5159,1.956752);
#1953=CIRCLE('',#5161,1.893248);
#1954=CIRCLE('',#5162,0.405071403305639);
#1955=CIRCLE('',#5164,0.405071403305639);
#1956=CIRCLE('',#5166,1.893248);
#1957=CIRCLE('',#5167,0.405071403305639);
#1958=CIRCLE('',#5169,0.405071403305639);
#1959=CIRCLE('',#5171,1.893248);
#1960=CIRCLE('',#5172,0.405071403305639);
#1961=CIRCLE('',#5174,0.405071403305639);
#1962=CIRCLE('',#5176,1.893248);
#1963=CIRCLE('',#5177,1.893248);
#1964=CIRCLE('',#5178,0.405071403305639);
#1965=CIRCLE('',#5180,0.405071403305639);
#1966=CIRCLE('',#5182,1.893248);
#1967=CIRCLE('',#5183,0.405071403305639);
#1968=CIRCLE('',#5185,0.405071403305639);
#1969=CIRCLE('',#5187,1.893248);
#1970=CIRCLE('',#5188,0.405071403305639);
#1971=CIRCLE('',#5190,0.405071403305639);
#1972=CIRCLE('',#5192,1.893248);
#1973=CIRCLE('',#5193,0.405071403305639);
#1974=CIRCLE('',#5195,0.405071403305639);
#1975=CIRCLE('',#5197,1.893248);
#1976=CIRCLE('',#5198,1.893248);
#1977=CIRCLE('',#5199,1.893248);
#1978=CIRCLE('',#5201,0.405071403305639);
#1979=CIRCLE('',#5203,0.405071403305639);
#1980=CIRCLE('',#5208,1.95469);
#1981=CIRCLE('',#5209,1.90031);
#1982=CIRCLE('',#5211,1.95469);
#1983=CIRCLE('',#5213,1.90031);
#1984=CIRCLE('',#5216,1.95469);
#1985=CIRCLE('',#5217,1.90031);
#1986=CIRCLE('',#5219,1.95469);
#1987=CIRCLE('',#5221,1.90031);
#1988=CIRCLE('',#5230,0.24505);
#1989=CIRCLE('',#5239,0.22);
#1990=CIRCLE('',#5241,0.24505);
#1991=CIRCLE('',#5246,0.165);
#1992=CIRCLE('',#5247,0.165);
#1993=CIRCLE('',#5250,0.165);
#1994=CIRCLE('',#5251,0.165);
#1995=CIRCLE('',#5254,0.165);
#1996=CIRCLE('',#5255,0.165);
#1997=CIRCLE('',#5258,0.165);
#1998=CIRCLE('',#5259,0.165);
#1999=CIRCLE('',#5262,0.31);
#2000=CIRCLE('',#5263,0.31);
#2001=CIRCLE('',#5266,0.31);
#2002=CIRCLE('',#5267,0.31);
#2003=CIRCLE('',#5270,0.31);
#2004=CIRCLE('',#5271,0.31);
#2005=CIRCLE('',#5274,0.31);
#2006=CIRCLE('',#5275,0.31);
#2007=CIRCLE('',#5278,0.31);
#2008=CIRCLE('',#5279,0.31);
#2009=CIRCLE('',#5282,0.31);
#2010=CIRCLE('',#5283,0.31);
#2011=CIRCLE('',#5286,0.31);
#2012=CIRCLE('',#5287,0.31);
#2013=CIRCLE('',#5290,0.31);
#2014=CIRCLE('',#5291,0.31);
#2015=CIRCLE('',#5294,0.31);
#2016=CIRCLE('',#5295,0.31);
#2017=CIRCLE('',#5298,0.31);
#2018=CIRCLE('',#5299,0.31);
#2019=CIRCLE('',#5302,0.31);
#2020=CIRCLE('',#5303,0.31);
#2021=CIRCLE('',#5306,0.31);
#2022=CIRCLE('',#5307,0.31);
#2023=CIRCLE('',#5310,0.165);
#2024=CIRCLE('',#5311,0.165);
#2025=CIRCLE('',#5314,0.165);
#2026=CIRCLE('',#5315,0.165);
#2027=CIRCLE('',#5318,0.165);
#2028=CIRCLE('',#5319,0.165);
#2029=CIRCLE('',#5322,0.165);
#2030=CIRCLE('',#5323,0.165);
#2031=CIRCLE('',#5326,0.33);
#2032=CIRCLE('',#5327,0.33);
#2033=CIRCLE('',#5329,0.33);
#2034=CIRCLE('',#5330,0.33);
#2035=CIRCLE('',#5332,0.33);
#2036=CIRCLE('',#5333,0.33);
#2037=CIRCLE('',#5335,0.33);
#2038=CIRCLE('',#5336,0.33);
#2039=CIRCLE('',#5338,0.33);
#2040=CIRCLE('',#5339,0.33);
#2041=CIRCLE('',#5341,0.33);
#2042=CIRCLE('',#5342,0.33);
#2043=CIRCLE('',#5344,0.33);
#2044=CIRCLE('',#5345,0.33);
#2045=CIRCLE('',#5347,0.33);
#2046=CIRCLE('',#5348,0.33);
#2047=CIRCLE('',#5350,2.);
#2048=CIRCLE('',#5351,1.9);
#2049=CIRCLE('',#5353,1.9);
#2050=CIRCLE('',#5355,2.6);
#2051=CIRCLE('',#5357,10.);
#2052=CIRCLE('',#5358,4.);
#2053=CIRCLE('',#5360,2.);
#2054=CIRCLE('',#5362,10.);
#2055=CIRCLE('',#5365,2.6);
#2056=CIRCLE('',#5367,4.);
#2057=CIRCLE('',#5371,2.);
#2058=CIRCLE('',#5372,2.);
#2059=CIRCLE('',#5374,2.59);
#2060=CIRCLE('',#5375,2.59);
#2061=CIRCLE('',#5380,0.225);
#2062=CIRCLE('',#5381,0.225);
#2063=CIRCLE('',#5383,0.225);
#2064=CIRCLE('',#5384,0.225);
#2065=CIRCLE('',#5386,0.225);
#2066=CIRCLE('',#5387,0.225);
#2067=CIRCLE('',#5389,0.225);
#2068=CIRCLE('',#5390,0.225);
#2069=CIRCLE('',#5392,2.59);
#2070=CIRCLE('',#5393,2.59);
#2071=CIRCLE('',#5395,1.9);
#2072=CIRCLE('',#5397,1.9);
#2073=CIRCLE('',#5399,4.);
#2074=CIRCLE('',#5400,4.);
#2075=CIRCLE('',#5405,0.225);
#2076=CIRCLE('',#5406,0.225);
#2077=CIRCLE('',#5408,0.225);
#2078=CIRCLE('',#5409,0.225);
#2079=CIRCLE('',#5411,0.225);
#2080=CIRCLE('',#5412,0.225);
#2081=CIRCLE('',#5414,0.225);
#2082=CIRCLE('',#5415,0.225);
#2083=CIRCLE('',#5417,0.31);
#2084=CIRCLE('',#5418,0.31);
#2085=CIRCLE('',#5420,0.31);
#2086=CIRCLE('',#5421,0.31);
#2087=CIRCLE('',#5423,0.31);
#2088=CIRCLE('',#5424,0.31);
#2089=CIRCLE('',#5426,0.31);
#2090=CIRCLE('',#5427,0.31);
#2091=CIRCLE('',#5429,0.31);
#2092=CIRCLE('',#5430,0.31);
#2093=CIRCLE('',#5432,0.31);
#2094=CIRCLE('',#5433,0.31);
#2095=CIRCLE('',#5435,0.31);
#2096=CIRCLE('',#5436,0.31);
#2097=CIRCLE('',#5438,0.31);
#2098=CIRCLE('',#5439,0.31);
#2099=CIRCLE('',#5441,0.31);
#2100=CIRCLE('',#5442,0.31);
#2101=CIRCLE('',#5444,0.31);
#2102=CIRCLE('',#5445,0.31);
#2103=CIRCLE('',#5447,0.31);
#2104=CIRCLE('',#5448,0.31);
#2105=CIRCLE('',#5450,0.31);
#2106=CIRCLE('',#5451,0.31);
#2107=CIRCLE('',#5453,6.5);
#2108=CIRCLE('',#5454,6.5);
#2109=CIRCLE('',#5456,8.);
#2110=CIRCLE('',#5457,8.);
#2111=CIRCLE('',#5462,0.3);
#2112=CIRCLE('',#5464,0.35);
#2113=CIRCLE('',#5466,0.35);
#2114=CIRCLE('',#5468,0.32);
#2115=CIRCLE('',#5470,0.22);
#2116=CIRCLE('',#5472,0.1954);
#2117=CIRCLE('',#5474,0.1954);
#2118=CIRCLE('',#5476,0.16);
#2119=CIRCLE('',#5524,0.3);
#2120=CIRCLE('',#5526,0.5);
#2121=CIRCLE('',#5527,0.3);
#2122=CIRCLE('',#5529,0.5);
#2123=CIRCLE('',#5530,0.3);
#2124=CIRCLE('',#5534,0.3);
#2125=CIRCLE('',#5538,0.21);
#2126=CIRCLE('',#5540,0.21);
#2127=CIRCLE('',#5543,0.3);
#2128=CIRCLE('',#5544,0.3);
#2129=CIRCLE('',#5546,1.2);
#2130=CIRCLE('',#5547,1.2);
#2131=CIRCLE('',#5559,0.22);
#2132=CIRCLE('',#5561,0.24505);
#2133=CIRCLE('',#5563,0.24505);
#2134=CIRCLE('',#5565,0.175);
#2135=VERTEX_POINT('',#7129);
#2136=VERTEX_POINT('',#7131);
#2137=VERTEX_POINT('',#7135);
#2138=VERTEX_POINT('',#7137);
#2139=VERTEX_POINT('',#7141);
#2140=VERTEX_POINT('',#7143);
#2141=VERTEX_POINT('',#7147);
#2142=VERTEX_POINT('',#7149);
#2143=VERTEX_POINT('',#7153);
#2144=VERTEX_POINT('',#7155);
#2145=VERTEX_POINT('',#7159);
#2146=VERTEX_POINT('',#7161);
#2147=VERTEX_POINT('',#7165);
#2148=VERTEX_POINT('',#7167);
#2149=VERTEX_POINT('',#7171);
#2150=VERTEX_POINT('',#7172);
#2151=VERTEX_POINT('',#7174);
#2152=VERTEX_POINT('',#7176);
#2153=VERTEX_POINT('',#7180);
#2154=VERTEX_POINT('',#7182);
#2155=VERTEX_POINT('',#7186);
#2156=VERTEX_POINT('',#7188);
#2157=VERTEX_POINT('',#7198);
#2158=VERTEX_POINT('',#7200);
#2159=VERTEX_POINT('',#7207);
#2160=VERTEX_POINT('',#7209);
#2161=VERTEX_POINT('',#7216);
#2162=VERTEX_POINT('',#7218);
#2163=VERTEX_POINT('',#7225);
#2164=VERTEX_POINT('',#7227);
#2165=VERTEX_POINT('',#7234);
#2166=VERTEX_POINT('',#7236);
#2167=VERTEX_POINT('',#7240);
#2168=VERTEX_POINT('',#7242);
#2169=VERTEX_POINT('',#7246);
#2170=VERTEX_POINT('',#7248);
#2171=VERTEX_POINT('',#7252);
#2172=VERTEX_POINT('',#7254);
#2173=VERTEX_POINT('',#7258);
#2174=VERTEX_POINT('',#7260);
#2175=VERTEX_POINT('',#7263);
#2176=VERTEX_POINT('',#7265);
#2177=VERTEX_POINT('',#7270);
#2178=VERTEX_POINT('',#7274);
#2179=VERTEX_POINT('',#7277);
#2180=VERTEX_POINT('',#7281);
#2181=VERTEX_POINT('',#7288);
#2182=VERTEX_POINT('',#7290);
#2183=VERTEX_POINT('',#7294);
#2184=VERTEX_POINT('',#7296);
#2185=VERTEX_POINT('',#7303);
#2186=VERTEX_POINT('',#7304);
#2187=VERTEX_POINT('',#7308);
#2188=VERTEX_POINT('',#7323);
#2189=VERTEX_POINT('',#7325);
#2190=VERTEX_POINT('',#7334);
#2191=VERTEX_POINT('',#7336);
#2192=VERTEX_POINT('',#7384);
#2193=VERTEX_POINT('',#7386);
#2194=VERTEX_POINT('',#7390);
#2195=VERTEX_POINT('',#7392);
#2196=VERTEX_POINT('',#7399);
#2197=VERTEX_POINT('',#7401);
#2198=VERTEX_POINT('',#7405);
#2199=VERTEX_POINT('',#7407);
#2200=VERTEX_POINT('',#7411);
#2201=VERTEX_POINT('',#7413);
#2202=VERTEX_POINT('',#7417);
#2203=VERTEX_POINT('',#7420);
#2204=VERTEX_POINT('',#7424);
#2205=VERTEX_POINT('',#7426);
#2206=VERTEX_POINT('',#7433);
#2207=VERTEX_POINT('',#7435);
#2208=VERTEX_POINT('',#7439);
#2209=VERTEX_POINT('',#7442);
#2210=VERTEX_POINT('',#7446);
#2211=VERTEX_POINT('',#7448);
#2212=VERTEX_POINT('',#8414);
#2213=VERTEX_POINT('',#8416);
#2214=VERTEX_POINT('',#8518);
#2215=VERTEX_POINT('',#8520);
#2216=VERTEX_POINT('',#8524);
#2217=VERTEX_POINT('',#8526);
#2218=VERTEX_POINT('',#8533);
#2219=VERTEX_POINT('',#8534);
#2220=VERTEX_POINT('',#8536);
#2221=VERTEX_POINT('',#8538);
#2222=VERTEX_POINT('',#8542);
#2223=VERTEX_POINT('',#8544);
#2224=VERTEX_POINT('',#8548);
#2225=VERTEX_POINT('',#8550);
#2226=VERTEX_POINT('',#8554);
#2227=VERTEX_POINT('',#8556);
#2228=VERTEX_POINT('',#8560);
#2229=VERTEX_POINT('',#8562);
#2230=VERTEX_POINT('',#8571);
#2231=VERTEX_POINT('',#8574);
#2232=VERTEX_POINT('',#8577);
#2233=VERTEX_POINT('',#8581);
#2234=VERTEX_POINT('',#8585);
#2235=VERTEX_POINT('',#8589);
#2236=VERTEX_POINT('',#8592);
#2237=VERTEX_POINT('',#8600);
#2238=VERTEX_POINT('',#8601);
#2239=VERTEX_POINT('',#8604);
#2240=VERTEX_POINT('',#8606);
#2241=VERTEX_POINT('',#8610);
#2242=VERTEX_POINT('',#8614);
#2243=VERTEX_POINT('',#8616);
#2244=VERTEX_POINT('',#8620);
#2245=VERTEX_POINT('',#8625);
#2246=VERTEX_POINT('',#8629);
#2247=VERTEX_POINT('',#8635);
#2248=VERTEX_POINT('',#8636);
#2249=VERTEX_POINT('',#8639);
#2250=VERTEX_POINT('',#8641);
#2251=VERTEX_POINT('',#8645);
#2252=VERTEX_POINT('',#8649);
#2253=VERTEX_POINT('',#8651);
#2254=VERTEX_POINT('',#8654);
#2255=VERTEX_POINT('',#8658);
#2256=VERTEX_POINT('',#8662);
#2257=VERTEX_POINT('',#8670);
#2258=VERTEX_POINT('',#8671);
#2259=VERTEX_POINT('',#8674);
#2260=VERTEX_POINT('',#8675);
#2261=VERTEX_POINT('',#8678);
#2262=VERTEX_POINT('',#8679);
#2263=VERTEX_POINT('',#8682);
#2264=VERTEX_POINT('',#8683);
#2265=VERTEX_POINT('',#8686);
#2266=VERTEX_POINT('',#8687);
#2267=VERTEX_POINT('',#8690);
#2268=VERTEX_POINT('',#8691);
#2269=VERTEX_POINT('',#8694);
#2270=VERTEX_POINT('',#8695);
#2271=VERTEX_POINT('',#8698);
#2272=VERTEX_POINT('',#8699);
#2273=VERTEX_POINT('',#8702);
#2274=VERTEX_POINT('',#8703);
#2275=VERTEX_POINT('',#8707);
#2276=VERTEX_POINT('',#8708);
#2277=VERTEX_POINT('',#8731);
#2278=VERTEX_POINT('',#8733);
#2279=VERTEX_POINT('',#8758);
#2280=VERTEX_POINT('',#8760);
#2281=VERTEX_POINT('',#8783);
#2282=VERTEX_POINT('',#8785);
#2283=VERTEX_POINT('',#8808);
#2284=VERTEX_POINT('',#8810);
#2285=VERTEX_POINT('',#8833);
#2286=VERTEX_POINT('',#8835);
#2287=VERTEX_POINT('',#8838);
#2288=VERTEX_POINT('',#8840);
#2289=VERTEX_POINT('',#8863);
#2290=VERTEX_POINT('',#8865);
#2291=VERTEX_POINT('',#8888);
#2292=VERTEX_POINT('',#8890);
#2293=VERTEX_POINT('',#8913);
#2294=VERTEX_POINT('',#8915);
#2295=VERTEX_POINT('',#8938);
#2296=VERTEX_POINT('',#8940);
#2297=VERTEX_POINT('',#8965);
#2298=VERTEX_POINT('',#8969);
#2299=VERTEX_POINT('',#8994);
#2300=VERTEX_POINT('',#8998);
#2301=VERTEX_POINT('',#9023);
#2302=VERTEX_POINT('',#9027);
#2303=VERTEX_POINT('',#9052);
#2304=VERTEX_POINT('',#9054);
#2305=VERTEX_POINT('',#9058);
#2306=VERTEX_POINT('',#9083);
#2307=VERTEX_POINT('',#9087);
#2308=VERTEX_POINT('',#9112);
#2309=VERTEX_POINT('',#9116);
#2310=VERTEX_POINT('',#9141);
#2311=VERTEX_POINT('',#9145);
#2312=VERTEX_POINT('',#9170);
#2313=VERTEX_POINT('',#9173);
#2314=VERTEX_POINT('',#9175);
#2315=VERTEX_POINT('',#9207);
#2316=VERTEX_POINT('',#9209);
#2317=VERTEX_POINT('',#9212);
#2318=VERTEX_POINT('',#9216);
#2319=VERTEX_POINT('',#9221);
#2320=VERTEX_POINT('',#9223);
#2321=VERTEX_POINT('',#9226);
#2322=VERTEX_POINT('',#9230);
#2323=VERTEX_POINT('',#9241);
#2324=VERTEX_POINT('',#9244);
#2325=VERTEX_POINT('',#9245);
#2326=VERTEX_POINT('',#9247);
#2327=VERTEX_POINT('',#9249);
#2328=VERTEX_POINT('',#9253);
#2329=VERTEX_POINT('',#9255);
#2330=VERTEX_POINT('',#9259);
#2331=VERTEX_POINT('',#9261);
#2332=VERTEX_POINT('',#9265);
#2333=VERTEX_POINT('',#9267);
#2334=VERTEX_POINT('',#9271);
#2335=VERTEX_POINT('',#9273);
#2336=VERTEX_POINT('',#9281);
#2337=VERTEX_POINT('',#9284);
#2338=VERTEX_POINT('',#9292);
#2339=VERTEX_POINT('',#9294);
#2340=VERTEX_POINT('',#9299);
#2341=VERTEX_POINT('',#9301);
#2342=VERTEX_POINT('',#9306);
#2343=VERTEX_POINT('',#9308);
#2344=VERTEX_POINT('',#9313);
#2345=VERTEX_POINT('',#9315);
#2346=VERTEX_POINT('',#9320);
#2347=VERTEX_POINT('',#9322);
#2348=VERTEX_POINT('',#9327);
#2349=VERTEX_POINT('',#9329);
#2350=VERTEX_POINT('',#9334);
#2351=VERTEX_POINT('',#9336);
#2352=VERTEX_POINT('',#9341);
#2353=VERTEX_POINT('',#9343);
#2354=VERTEX_POINT('',#9348);
#2355=VERTEX_POINT('',#9350);
#2356=VERTEX_POINT('',#9355);
#2357=VERTEX_POINT('',#9357);
#2358=VERTEX_POINT('',#9362);
#2359=VERTEX_POINT('',#9364);
#2360=VERTEX_POINT('',#9369);
#2361=VERTEX_POINT('',#9371);
#2362=VERTEX_POINT('',#9376);
#2363=VERTEX_POINT('',#9378);
#2364=VERTEX_POINT('',#9383);
#2365=VERTEX_POINT('',#9385);
#2366=VERTEX_POINT('',#9390);
#2367=VERTEX_POINT('',#9392);
#2368=VERTEX_POINT('',#9397);
#2369=VERTEX_POINT('',#9399);
#2370=VERTEX_POINT('',#9404);
#2371=VERTEX_POINT('',#9406);
#2372=VERTEX_POINT('',#9411);
#2373=VERTEX_POINT('',#9413);
#2374=VERTEX_POINT('',#9418);
#2375=VERTEX_POINT('',#9420);
#2376=VERTEX_POINT('',#9425);
#2377=VERTEX_POINT('',#9427);
#2378=VERTEX_POINT('',#9432);
#2379=VERTEX_POINT('',#9434);
#2380=VERTEX_POINT('',#9438);
#2381=VERTEX_POINT('',#9440);
#2382=VERTEX_POINT('',#9444);
#2383=VERTEX_POINT('',#9446);
#2384=VERTEX_POINT('',#9450);
#2385=VERTEX_POINT('',#9452);
#2386=VERTEX_POINT('',#9456);
#2387=VERTEX_POINT('',#9458);
#2388=VERTEX_POINT('',#9462);
#2389=VERTEX_POINT('',#9464);
#2390=VERTEX_POINT('',#9468);
#2391=VERTEX_POINT('',#9470);
#2392=VERTEX_POINT('',#9474);
#2393=VERTEX_POINT('',#9476);
#2394=VERTEX_POINT('',#9480);
#2395=VERTEX_POINT('',#9482);
#2396=VERTEX_POINT('',#9485);
#2397=VERTEX_POINT('',#9489);
#2398=VERTEX_POINT('',#9492);
#2399=VERTEX_POINT('',#9494);
#2400=VERTEX_POINT('',#9497);
#2401=VERTEX_POINT('',#9501);
#2402=VERTEX_POINT('',#9506);
#2403=VERTEX_POINT('',#9510);
#2404=VERTEX_POINT('',#9516);
#2405=VERTEX_POINT('',#9518);
#2406=VERTEX_POINT('',#9522);
#2407=VERTEX_POINT('',#9524);
#2408=VERTEX_POINT('',#9531);
#2409=VERTEX_POINT('',#9533);
#2410=VERTEX_POINT('',#9537);
#2411=VERTEX_POINT('',#9539);
#2412=VERTEX_POINT('',#9543);
#2413=VERTEX_POINT('',#9545);
#2414=VERTEX_POINT('',#9549);
#2415=VERTEX_POINT('',#9551);
#2416=VERTEX_POINT('',#9555);
#2417=VERTEX_POINT('',#9557);
#2418=VERTEX_POINT('',#9561);
#2419=VERTEX_POINT('',#9564);
#2420=VERTEX_POINT('',#9568);
#2421=VERTEX_POINT('',#9570);
#2422=VERTEX_POINT('',#9577);
#2423=VERTEX_POINT('',#9579);
#2424=VERTEX_POINT('',#9583);
#2425=VERTEX_POINT('',#9585);
#2426=VERTEX_POINT('',#9589);
#2427=VERTEX_POINT('',#9591);
#2428=VERTEX_POINT('',#9595);
#2429=VERTEX_POINT('',#9597);
#2430=VERTEX_POINT('',#9601);
#2431=VERTEX_POINT('',#9603);
#2432=VERTEX_POINT('',#9607);
#2433=VERTEX_POINT('',#9609);
#2434=VERTEX_POINT('',#9613);
#2435=VERTEX_POINT('',#9615);
#2436=VERTEX_POINT('',#9619);
#2437=VERTEX_POINT('',#9621);
#2438=VERTEX_POINT('',#9625);
#2439=VERTEX_POINT('',#9627);
#2440=VERTEX_POINT('',#9631);
#2441=VERTEX_POINT('',#9633);
#2442=VERTEX_POINT('',#9637);
#2443=VERTEX_POINT('',#9639);
#2444=VERTEX_POINT('',#9643);
#2445=VERTEX_POINT('',#9645);
#2446=VERTEX_POINT('',#9649);
#2447=VERTEX_POINT('',#9651);
#2448=VERTEX_POINT('',#9655);
#2449=VERTEX_POINT('',#9657);
#2450=VERTEX_POINT('',#9661);
#2451=VERTEX_POINT('',#9663);
#2452=VERTEX_POINT('',#9667);
#2453=VERTEX_POINT('',#9669);
#2454=VERTEX_POINT('',#9673);
#2455=VERTEX_POINT('',#9675);
#2456=VERTEX_POINT('',#9679);
#2457=VERTEX_POINT('',#9681);
#2458=VERTEX_POINT('',#9688);
#2459=VERTEX_POINT('',#9691);
#2460=VERTEX_POINT('',#9695);
#2461=VERTEX_POINT('',#9699);
#2462=VERTEX_POINT('',#9703);
#2463=VERTEX_POINT('',#9706);
#2464=VERTEX_POINT('',#9710);
#2465=VERTEX_POINT('',#9714);
#2466=VERTEX_POINT('',#9719);
#2467=VERTEX_POINT('',#9720);
#2468=VERTEX_POINT('',#9722);
#2469=VERTEX_POINT('',#9724);
#2470=VERTEX_POINT('',#9728);
#2471=VERTEX_POINT('',#9730);
#2472=VERTEX_POINT('',#9734);
#2473=VERTEX_POINT('',#9736);
#2474=VERTEX_POINT('',#9740);
#2475=VERTEX_POINT('',#9742);
#2476=VERTEX_POINT('',#9746);
#2477=VERTEX_POINT('',#9748);
#2478=VERTEX_POINT('',#9794);
#2479=VERTEX_POINT('',#9797);
#2480=VERTEX_POINT('',#9799);
#2481=VERTEX_POINT('',#9802);
#2482=VERTEX_POINT('',#9804);
#2483=VERTEX_POINT('',#9811);
#2484=VERTEX_POINT('',#9817);
#2485=VERTEX_POINT('',#9818);
#2486=VERTEX_POINT('',#9822);
#2487=VERTEX_POINT('',#9829);
#2488=VERTEX_POINT('',#9831);
#2489=VERTEX_POINT('',#9836);
#2490=VERTEX_POINT('',#9838);
#2491=VERTEX_POINT('',#9882);
#2492=VERTEX_POINT('',#9884);
#2493=VERTEX_POINT('',#9888);
#2494=VERTEX_POINT('',#9890);
#2495=VERTEX_POINT('',#9897);
#2496=VERTEX_POINT('',#9898);
#2497=VERTEX_POINT('',#9900);
#2498=VERTEX_POINT('',#9902);
#2499=VERTEX_POINT('',#9906);
#2500=VERTEX_POINT('',#9908);
#2501=VERTEX_POINT('',#9912);
#2502=VERTEX_POINT('',#9914);
#2503=VERTEX_POINT('',#9918);
#2504=VERTEX_POINT('',#9920);
#2505=VERTEX_POINT('',#9924);
#2506=VERTEX_POINT('',#9926);
#2507=VERTEX_POINT('',#9934);
#2508=VERTEX_POINT('',#9937);
#2509=VERTEX_POINT('',#9941);
#2510=VERTEX_POINT('',#9945);
#2511=EDGE_CURVE('',#2135,#2135,#1832,.T.);
#2512=EDGE_CURVE('',#2135,#2136,#1392,.T.);
#2513=EDGE_CURVE('',#2136,#2136,#1833,.T.);
#2514=EDGE_CURVE('',#2137,#2137,#1834,.T.);
#2515=EDGE_CURVE('',#2137,#2138,#1393,.T.);
#2516=EDGE_CURVE('',#2138,#2138,#1835,.T.);
#2517=EDGE_CURVE('',#2139,#2139,#1836,.T.);
#2518=EDGE_CURVE('',#2139,#2140,#1394,.T.);
#2519=EDGE_CURVE('',#2140,#2140,#1837,.T.);
#2520=EDGE_CURVE('',#2141,#2141,#1838,.T.);
#2521=EDGE_CURVE('',#2141,#2142,#1395,.T.);
#2522=EDGE_CURVE('',#2142,#2142,#1839,.T.);
#2523=EDGE_CURVE('',#2143,#2143,#1840,.T.);
#2524=EDGE_CURVE('',#2143,#2144,#1396,.T.);
#2525=EDGE_CURVE('',#2144,#2144,#1841,.T.);
#2526=EDGE_CURVE('',#2145,#2145,#1842,.T.);
#2527=EDGE_CURVE('',#2145,#2146,#1397,.T.);
#2528=EDGE_CURVE('',#2146,#2146,#1843,.T.);
#2529=EDGE_CURVE('',#2147,#2147,#1844,.T.);
#2530=EDGE_CURVE('',#2147,#2148,#1398,.T.);
#2531=EDGE_CURVE('',#2148,#2148,#1845,.T.);
#2532=EDGE_CURVE('',#2149,#2150,#1399,.T.);
#2533=EDGE_CURVE('',#2150,#2151,#1400,.T.);
#2534=EDGE_CURVE('',#2152,#2151,#1401,.T.);
#2535=EDGE_CURVE('',#2149,#2152,#1402,.T.);
#2536=EDGE_CURVE('',#2153,#2149,#1403,.T.);
#2537=EDGE_CURVE('',#2154,#2152,#1404,.T.);
#2538=EDGE_CURVE('',#2153,#2154,#1405,.T.);
#2539=EDGE_CURVE('',#2155,#2153,#1406,.T.);
#2540=EDGE_CURVE('',#2156,#2154,#1407,.T.);
#2541=EDGE_CURVE('',#2155,#2156,#1408,.T.);
#2542=EDGE_CURVE('',#2150,#2155,#1409,.T.);
#2543=EDGE_CURVE('',#2151,#2156,#1410,.T.);
#2544=EDGE_CURVE('',#2157,#2157,#1846,.T.);
#2545=EDGE_CURVE('',#2157,#2158,#1411,.T.);
#2546=EDGE_CURVE('',#2158,#2158,#1847,.T.);
#2547=EDGE_CURVE('',#2159,#2159,#1848,.T.);
#2548=EDGE_CURVE('',#2159,#2160,#1412,.T.);
#2549=EDGE_CURVE('',#2160,#2160,#1849,.T.);
#2550=EDGE_CURVE('',#2161,#2161,#1850,.T.);
#2551=EDGE_CURVE('',#2161,#2162,#1413,.T.);
#2552=EDGE_CURVE('',#2162,#2162,#1851,.T.);
#2553=EDGE_CURVE('',#2163,#2163,#1852,.T.);
#2554=EDGE_CURVE('',#2163,#2164,#1414,.T.);
#2555=EDGE_CURVE('',#2164,#2164,#1853,.T.);
#2556=EDGE_CURVE('',#2165,#2165,#1854,.T.);
#2557=EDGE_CURVE('',#2165,#2166,#1415,.T.);
#2558=EDGE_CURVE('',#2166,#2166,#1855,.T.);
#2559=EDGE_CURVE('',#2167,#2167,#1856,.T.);
#2560=EDGE_CURVE('',#2167,#2168,#1416,.T.);
#2561=EDGE_CURVE('',#2168,#2168,#1857,.T.);
#2562=EDGE_CURVE('',#2169,#2169,#1858,.T.);
#2563=EDGE_CURVE('',#2169,#2170,#1417,.T.);
#2564=EDGE_CURVE('',#2170,#2170,#1859,.T.);
#2565=EDGE_CURVE('',#2171,#2171,#1860,.T.);
#2566=EDGE_CURVE('',#2171,#2172,#1418,.T.);
#2567=EDGE_CURVE('',#2172,#2172,#1861,.T.);
#2568=EDGE_CURVE('',#2173,#2173,#1862,.T.);
#2569=EDGE_CURVE('',#2174,#2174,#1863,.T.);
#2570=EDGE_CURVE('',#2175,#2175,#1864,.T.);
#2571=EDGE_CURVE('',#2176,#2176,#1865,.T.);
#2572=EDGE_CURVE('',#2173,#2175,#1419,.T.);
#2573=EDGE_CURVE('',#2176,#2177,#1420,.T.);
#2574=EDGE_CURVE('',#2177,#2177,#1866,.T.);
#2575=EDGE_CURVE('',#2178,#2178,#1867,.T.);
#2576=EDGE_CURVE('',#2178,#2179,#1421,.T.);
#2577=EDGE_CURVE('',#2179,#2179,#1868,.T.);
#2578=EDGE_CURVE('',#2180,#2180,#1869,.T.);
#2579=EDGE_CURVE('',#2180,#2174,#1422,.T.);
#2580=EDGE_CURVE('',#2181,#2181,#1870,.T.);
#2581=EDGE_CURVE('',#2181,#2182,#1423,.T.);
#2582=EDGE_CURVE('',#2182,#2182,#1871,.T.);
#2583=EDGE_CURVE('',#2183,#2183,#1872,.T.);
#2584=EDGE_CURVE('',#2183,#2184,#1424,.T.);
#2585=EDGE_CURVE('',#2184,#2184,#1873,.T.);
#2586=EDGE_CURVE('',#2185,#2186,#1425,.T.);
#2587=EDGE_CURVE('',#2185,#2186,#1874,.T.);
#2588=EDGE_CURVE('',#2187,#2185,#234,.T.);
#2589=EDGE_CURVE('',#2188,#2187,#1875,.T.);
#2590=EDGE_CURVE('',#2189,#2188,#235,.T.);
#2591=EDGE_CURVE('',#2189,#2190,#1426,.T.);
#2592=EDGE_CURVE('',#2191,#2190,#236,.T.);
#2593=EDGE_CURVE('',#2190,#2191,#237,.T.);
#2594=EDGE_CURVE('',#2186,#2189,#238,.T.);
#2595=EDGE_CURVE('',#2188,#2187,#1427,.T.);
#2596=EDGE_CURVE('',#2192,#2192,#1876,.T.);
#2597=EDGE_CURVE('',#2192,#2193,#1428,.T.);
#2598=EDGE_CURVE('',#2193,#2193,#1877,.T.);
#2599=EDGE_CURVE('',#2194,#2194,#1878,.T.);
#2600=EDGE_CURVE('',#2194,#2195,#1429,.T.);
#2601=EDGE_CURVE('',#2195,#2195,#1879,.T.);
#2602=EDGE_CURVE('',#2196,#2196,#1880,.T.);
#2603=EDGE_CURVE('',#2196,#2197,#1430,.T.);
#2604=EDGE_CURVE('',#2197,#2197,#1881,.T.);
#2605=EDGE_CURVE('',#2198,#2198,#1882,.T.);
#2606=EDGE_CURVE('',#2198,#2199,#1431,.T.);
#2607=EDGE_CURVE('',#2199,#2199,#1883,.T.);
#2608=EDGE_CURVE('',#2200,#2200,#1884,.T.);
#2609=EDGE_CURVE('',#2200,#2201,#1432,.T.);
#2610=EDGE_CURVE('',#2201,#2201,#1885,.T.);
#2611=EDGE_CURVE('',#2202,#2202,#1886,.T.);
#2612=EDGE_CURVE('',#2202,#2203,#1433,.T.);
#2613=EDGE_CURVE('',#2203,#2203,#1887,.T.);
#2614=EDGE_CURVE('',#2204,#2204,#1888,.T.);
#2615=EDGE_CURVE('',#2204,#2205,#1434,.T.);
#2616=EDGE_CURVE('',#2205,#2205,#1889,.T.);
#2617=EDGE_CURVE('',#2206,#2206,#1890,.T.);
#2618=EDGE_CURVE('',#2206,#2207,#1435,.T.);
#2619=EDGE_CURVE('',#2207,#2207,#1891,.T.);
#2620=EDGE_CURVE('',#2208,#2208,#1892,.T.);
#2621=EDGE_CURVE('',#2208,#2209,#1436,.T.);
#2622=EDGE_CURVE('',#2209,#2209,#1893,.T.);
#2623=EDGE_CURVE('',#2210,#2210,#1894,.T.);
#2624=EDGE_CURVE('',#2210,#2211,#1437,.T.);
#2625=EDGE_CURVE('',#2211,#2211,#1895,.T.);
#2626=EDGE_CURVE('',#2212,#2212,#1896,.T.);
#2627=EDGE_CURVE('',#2212,#2213,#239,.T.);
#2628=EDGE_CURVE('',#2213,#2213,#1897,.T.);
#2629=EDGE_CURVE('',#2214,#2214,#1898,.T.);
#2630=EDGE_CURVE('',#2214,#2215,#1438,.T.);
#2631=EDGE_CURVE('',#2215,#2215,#1899,.T.);
#2632=EDGE_CURVE('',#2216,#2216,#1900,.T.);
#2633=EDGE_CURVE('',#2216,#2217,#1439,.T.);
#2634=EDGE_CURVE('',#2217,#2217,#1901,.T.);
#2635=EDGE_CURVE('',#2218,#2219,#1440,.T.);
#2636=EDGE_CURVE('',#2219,#2220,#1441,.T.);
#2637=EDGE_CURVE('',#2220,#2221,#1442,.T.);
#2638=EDGE_CURVE('',#2218,#2221,#1443,.T.);
#2639=EDGE_CURVE('',#2219,#2222,#1444,.T.);
#2640=EDGE_CURVE('',#2222,#2223,#1445,.T.);
#2641=EDGE_CURVE('',#2223,#2220,#1446,.T.);
#2642=EDGE_CURVE('',#2222,#2224,#1447,.T.);
#2643=EDGE_CURVE('',#2224,#2225,#1448,.T.);
#2644=EDGE_CURVE('',#2225,#2223,#1449,.T.);
#2645=EDGE_CURVE('',#2224,#2226,#1450,.T.);
#2646=EDGE_CURVE('',#2226,#2227,#1451,.T.);
#2647=EDGE_CURVE('',#2227,#2225,#1452,.T.);
#2648=EDGE_CURVE('',#2226,#2228,#1453,.T.);
#2649=EDGE_CURVE('',#2228,#2229,#1454,.T.);
#2650=EDGE_CURVE('',#2229,#2227,#1455,.T.);
#2651=EDGE_CURVE('',#2228,#2218,#1456,.T.);
#2652=EDGE_CURVE('',#2221,#2229,#1457,.T.);
#2653=EDGE_CURVE('',#2230,#2230,#1902,.T.);
#2654=EDGE_CURVE('',#2231,#2231,#1903,.T.);
#2655=EDGE_CURVE('',#2232,#2232,#1904,.T.);
#2656=EDGE_CURVE('',#2232,#2231,#1458,.T.);
#2657=EDGE_CURVE('',#2233,#2233,#1905,.T.);
#2658=EDGE_CURVE('',#2233,#2232,#1459,.T.);
#2659=EDGE_CURVE('',#2234,#2234,#1906,.T.);
#2660=EDGE_CURVE('',#2234,#2233,#1460,.T.);
#2661=EDGE_CURVE('',#2235,#2235,#1907,.T.);
#2662=EDGE_CURVE('',#2236,#2236,#1908,.F.);
#2663=EDGE_CURVE('',#2236,#2235,#1461,.T.);
#2664=EDGE_CURVE('',#2230,#2236,#1462,.T.);
#2665=EDGE_CURVE('',#2237,#2238,#1909,.T.);
#2666=EDGE_CURVE('',#2238,#2237,#1910,.T.);
#2667=EDGE_CURVE('',#2238,#2239,#1911,.T.);
#2668=EDGE_CURVE('',#2240,#2239,#1912,.T.);
#2669=EDGE_CURVE('',#2239,#2240,#1913,.T.);
#2670=EDGE_CURVE('',#2240,#2241,#1463,.T.);
#2671=EDGE_CURVE('',#2241,#2241,#1914,.T.);
#2672=EDGE_CURVE('',#2242,#2242,#1915,.T.);
#2673=EDGE_CURVE('',#2242,#2243,#1464,.T.);
#2674=EDGE_CURVE('',#2243,#2243,#1916,.T.);
#2675=EDGE_CURVE('',#2243,#2244,#1465,.T.);
#2676=EDGE_CURVE('',#2244,#2244,#1917,.T.);
#2677=EDGE_CURVE('',#2245,#2245,#1918,.T.);
#2678=EDGE_CURVE('',#2245,#2237,#1466,.T.);
#2679=EDGE_CURVE('',#2246,#2246,#1919,.T.);
#2680=EDGE_CURVE('',#2246,#2242,#1467,.T.);
#2681=EDGE_CURVE('',#2247,#2248,#1920,.T.);
#2682=EDGE_CURVE('',#2248,#2247,#1921,.T.);
#2683=EDGE_CURVE('',#2248,#2249,#1922,.T.);
#2684=EDGE_CURVE('',#2250,#2249,#1923,.T.);
#2685=EDGE_CURVE('',#2249,#2250,#1924,.T.);
#2686=EDGE_CURVE('',#2251,#2251,#1925,.T.);
#2687=EDGE_CURVE('',#2251,#2250,#1468,.T.);
#2688=EDGE_CURVE('',#2252,#2252,#1926,.T.);
#2689=EDGE_CURVE('',#2253,#2253,#1927,.T.);
#2690=EDGE_CURVE('',#2254,#2254,#1928,.T.);
#2691=EDGE_CURVE('',#2254,#2252,#1469,.T.);
#2692=EDGE_CURVE('',#2255,#2255,#1929,.T.);
#2693=EDGE_CURVE('',#2255,#2254,#1470,.T.);
#2694=EDGE_CURVE('',#2256,#2256,#1930,.T.);
#2695=EDGE_CURVE('',#2256,#2255,#1471,.T.);
#2696=EDGE_CURVE('',#2247,#2253,#1472,.T.);
#2697=EDGE_CURVE('',#2257,#2258,#1931,.T.);
#2698=EDGE_CURVE('',#2259,#2260,#1932,.T.);
#2699=EDGE_CURVE('',#2261,#2262,#1933,.T.);
#2700=EDGE_CURVE('',#2263,#2264,#1934,.T.);
#2701=EDGE_CURVE('',#2265,#2266,#1935,.T.);
#2702=EDGE_CURVE('',#2267,#2268,#1936,.T.);
#2703=EDGE_CURVE('',#2269,#2270,#1937,.T.);
#2704=EDGE_CURVE('',#2271,#2272,#1938,.T.);
#2705=EDGE_CURVE('',#2273,#2274,#1939,.T.);
#2706=EDGE_CURVE('',#2275,#2276,#240,.T.);
#2707=EDGE_CURVE('',#2277,#2275,#1940,.T.);
#2708=EDGE_CURVE('',#2278,#2277,#241,.T.);
#2709=EDGE_CURVE('',#2276,#2278,#1941,.T.);
#2710=EDGE_CURVE('',#2279,#2277,#1942,.T.);
#2711=EDGE_CURVE('',#2279,#2280,#242,.T.);
#2712=EDGE_CURVE('',#2281,#2280,#1943,.T.);
#2713=EDGE_CURVE('',#2281,#2282,#243,.T.);
#2714=EDGE_CURVE('',#2283,#2282,#1944,.T.);
#2715=EDGE_CURVE('',#2283,#2284,#244,.T.);
#2716=EDGE_CURVE('',#2285,#2284,#1945,.T.);
#2717=EDGE_CURVE('',#2285,#2286,#1473,.T.);
#2718=EDGE_CURVE('',#2286,#2286,#1946,.T.);
#2719=EDGE_CURVE('',#2287,#2285,#1947,.T.);
#2720=EDGE_CURVE('',#2287,#2288,#245,.T.);
#2721=EDGE_CURVE('',#2289,#2288,#1948,.T.);
#2722=EDGE_CURVE('',#2289,#2290,#246,.T.);
#2723=EDGE_CURVE('',#2291,#2290,#1949,.T.);
#2724=EDGE_CURVE('',#2291,#2292,#247,.T.);
#2725=EDGE_CURVE('',#2293,#2292,#1950,.T.);
#2726=EDGE_CURVE('',#2293,#2294,#248,.T.);
#2727=EDGE_CURVE('',#2295,#2294,#1951,.T.);
#2728=EDGE_CURVE('',#2295,#2296,#249,.T.);
#2729=EDGE_CURVE('',#2278,#2296,#1952,.T.);
#2730=EDGE_CURVE('',#2275,#2297,#1953,.T.);
#2731=EDGE_CURVE('',#2297,#2279,#1954,.T.);
#2732=EDGE_CURVE('',#2298,#2297,#250,.T.);
#2733=EDGE_CURVE('',#2280,#2298,#1955,.T.);
#2734=EDGE_CURVE('',#2298,#2299,#1956,.T.);
#2735=EDGE_CURVE('',#2299,#2281,#1957,.T.);
#2736=EDGE_CURVE('',#2300,#2299,#251,.T.);
#2737=EDGE_CURVE('',#2282,#2300,#1958,.T.);
#2738=EDGE_CURVE('',#2300,#2301,#1959,.T.);
#2739=EDGE_CURVE('',#2301,#2283,#1960,.T.);
#2740=EDGE_CURVE('',#2302,#2301,#252,.T.);
#2741=EDGE_CURVE('',#2284,#2302,#1961,.T.);
#2742=EDGE_CURVE('',#2302,#2303,#1962,.T.);
#2743=EDGE_CURVE('',#2303,#2304,#1963,.T.);
#2744=EDGE_CURVE('',#2304,#2287,#1964,.T.);
#2745=EDGE_CURVE('',#2305,#2304,#253,.T.);
#2746=EDGE_CURVE('',#2288,#2305,#1965,.T.);
#2747=EDGE_CURVE('',#2305,#2306,#1966,.T.);
#2748=EDGE_CURVE('',#2306,#2289,#1967,.T.);
#2749=EDGE_CURVE('',#2307,#2306,#254,.T.);
#2750=EDGE_CURVE('',#2290,#2307,#1968,.T.);
#2751=EDGE_CURVE('',#2307,#2308,#1969,.T.);
#2752=EDGE_CURVE('',#2308,#2291,#1970,.T.);
#2753=EDGE_CURVE('',#2309,#2308,#255,.T.);
#2754=EDGE_CURVE('',#2292,#2309,#1971,.T.);
#2755=EDGE_CURVE('',#2309,#2310,#1972,.T.);
#2756=EDGE_CURVE('',#2310,#2293,#1973,.T.);
#2757=EDGE_CURVE('',#2311,#2310,#256,.T.);
#2758=EDGE_CURVE('',#2294,#2311,#1974,.T.);
#2759=EDGE_CURVE('',#2312,#2312,#1975,.T.);
#2760=EDGE_CURVE('',#2312,#2303,#1474,.T.);
#2761=EDGE_CURVE('',#2313,#2276,#1976,.T.);
#2762=EDGE_CURVE('',#2313,#2314,#257,.T.);
#2763=EDGE_CURVE('',#2311,#2314,#1977,.T.);
#2764=EDGE_CURVE('',#2296,#2313,#1978,.T.);
#2765=EDGE_CURVE('',#2314,#2295,#1979,.T.);
#2766=EDGE_CURVE('',#2315,#2315,#1980,.T.);
#2767=EDGE_CURVE('',#2316,#2316,#1981,.T.);
#2768=EDGE_CURVE('',#2317,#2317,#1982,.T.);
#2769=EDGE_CURVE('',#2317,#2315,#1475,.T.);
#2770=EDGE_CURVE('',#2318,#2318,#1983,.T.);
#2771=EDGE_CURVE('',#2318,#2316,#1476,.T.);
#2772=EDGE_CURVE('',#2319,#2319,#1984,.T.);
#2773=EDGE_CURVE('',#2320,#2320,#1985,.T.);
#2774=EDGE_CURVE('',#2321,#2321,#1986,.T.);
#2775=EDGE_CURVE('',#2321,#2319,#1477,.T.);
#2776=EDGE_CURVE('',#2322,#2322,#1987,.T.);
#2777=EDGE_CURVE('',#2322,#2320,#1478,.T.);
#2778=EDGE_CURVE('',#2323,#2323,#1988,.T.);
#2779=EDGE_CURVE('',#2324,#2325,#1479,.T.);
#2780=EDGE_CURVE('',#2324,#2326,#1480,.T.);
#2781=EDGE_CURVE('',#2326,#2327,#1481,.T.);
#2782=EDGE_CURVE('',#2325,#2327,#1482,.T.);
#2783=EDGE_CURVE('',#2328,#2324,#1483,.T.);
#2784=EDGE_CURVE('',#2328,#2329,#1484,.T.);
#2785=EDGE_CURVE('',#2329,#2326,#1485,.T.);
#2786=EDGE_CURVE('',#2330,#2328,#1486,.T.);
#2787=EDGE_CURVE('',#2330,#2331,#1487,.T.);
#2788=EDGE_CURVE('',#2331,#2329,#1488,.T.);
#2789=EDGE_CURVE('',#2332,#2330,#1489,.T.);
#2790=EDGE_CURVE('',#2332,#2333,#1490,.T.);
#2791=EDGE_CURVE('',#2333,#2331,#1491,.T.);
#2792=EDGE_CURVE('',#2334,#2332,#1492,.T.);
#2793=EDGE_CURVE('',#2334,#2335,#1493,.T.);
#2794=EDGE_CURVE('',#2335,#2333,#1494,.T.);
#2795=EDGE_CURVE('',#2325,#2334,#1495,.T.);
#2796=EDGE_CURVE('',#2327,#2335,#1496,.T.);
#2797=EDGE_CURVE('',#2336,#2336,#1989,.T.);
#2798=EDGE_CURVE('',#2337,#2337,#1990,.T.);
#2799=EDGE_CURVE('',#2337,#2336,#1497,.T.);
#2800=EDGE_CURVE('',#2323,#2337,#1498,.T.);
#2801=EDGE_CURVE('',#2338,#2338,#1991,.T.);
#2802=EDGE_CURVE('',#2338,#2339,#1499,.T.);
#2803=EDGE_CURVE('',#2339,#2339,#1992,.T.);
#2804=EDGE_CURVE('',#2340,#2340,#1993,.T.);
#2805=EDGE_CURVE('',#2340,#2341,#1500,.T.);
#2806=EDGE_CURVE('',#2341,#2341,#1994,.T.);
#2807=EDGE_CURVE('',#2342,#2342,#1995,.T.);
#2808=EDGE_CURVE('',#2342,#2343,#1501,.T.);
#2809=EDGE_CURVE('',#2343,#2343,#1996,.T.);
#2810=EDGE_CURVE('',#2344,#2344,#1997,.T.);
#2811=EDGE_CURVE('',#2344,#2345,#1502,.T.);
#2812=EDGE_CURVE('',#2345,#2345,#1998,.T.);
#2813=EDGE_CURVE('',#2346,#2346,#1999,.T.);
#2814=EDGE_CURVE('',#2346,#2347,#1503,.T.);
#2815=EDGE_CURVE('',#2347,#2347,#2000,.T.);
#2816=EDGE_CURVE('',#2348,#2348,#2001,.T.);
#2817=EDGE_CURVE('',#2348,#2349,#1504,.T.);
#2818=EDGE_CURVE('',#2349,#2349,#2002,.T.);
#2819=EDGE_CURVE('',#2350,#2350,#2003,.T.);
#2820=EDGE_CURVE('',#2350,#2351,#1505,.T.);
#2821=EDGE_CURVE('',#2351,#2351,#2004,.T.);
#2822=EDGE_CURVE('',#2352,#2352,#2005,.T.);
#2823=EDGE_CURVE('',#2352,#2353,#1506,.T.);
#2824=EDGE_CURVE('',#2353,#2353,#2006,.T.);
#2825=EDGE_CURVE('',#2354,#2354,#2007,.T.);
#2826=EDGE_CURVE('',#2354,#2355,#1507,.T.);
#2827=EDGE_CURVE('',#2355,#2355,#2008,.T.);
#2828=EDGE_CURVE('',#2356,#2356,#2009,.T.);
#2829=EDGE_CURVE('',#2356,#2357,#1508,.T.);
#2830=EDGE_CURVE('',#2357,#2357,#2010,.T.);
#2831=EDGE_CURVE('',#2358,#2358,#2011,.T.);
#2832=EDGE_CURVE('',#2358,#2359,#1509,.T.);
#2833=EDGE_CURVE('',#2359,#2359,#2012,.T.);
#2834=EDGE_CURVE('',#2360,#2360,#2013,.T.);
#2835=EDGE_CURVE('',#2360,#2361,#1510,.T.);
#2836=EDGE_CURVE('',#2361,#2361,#2014,.T.);
#2837=EDGE_CURVE('',#2362,#2362,#2015,.T.);
#2838=EDGE_CURVE('',#2362,#2363,#1511,.T.);
#2839=EDGE_CURVE('',#2363,#2363,#2016,.T.);
#2840=EDGE_CURVE('',#2364,#2364,#2017,.T.);
#2841=EDGE_CURVE('',#2364,#2365,#1512,.T.);
#2842=EDGE_CURVE('',#2365,#2365,#2018,.T.);
#2843=EDGE_CURVE('',#2366,#2366,#2019,.T.);
#2844=EDGE_CURVE('',#2366,#2367,#1513,.T.);
#2845=EDGE_CURVE('',#2367,#2367,#2020,.T.);
#2846=EDGE_CURVE('',#2368,#2368,#2021,.T.);
#2847=EDGE_CURVE('',#2368,#2369,#1514,.T.);
#2848=EDGE_CURVE('',#2369,#2369,#2022,.T.);
#2849=EDGE_CURVE('',#2370,#2370,#2023,.T.);
#2850=EDGE_CURVE('',#2370,#2371,#1515,.T.);
#2851=EDGE_CURVE('',#2371,#2371,#2024,.T.);
#2852=EDGE_CURVE('',#2372,#2372,#2025,.T.);
#2853=EDGE_CURVE('',#2372,#2373,#1516,.T.);
#2854=EDGE_CURVE('',#2373,#2373,#2026,.T.);
#2855=EDGE_CURVE('',#2374,#2374,#2027,.T.);
#2856=EDGE_CURVE('',#2374,#2375,#1517,.T.);
#2857=EDGE_CURVE('',#2375,#2375,#2028,.T.);
#2858=EDGE_CURVE('',#2376,#2376,#2029,.T.);
#2859=EDGE_CURVE('',#2376,#2377,#1518,.T.);
#2860=EDGE_CURVE('',#2377,#2377,#2030,.T.);
#2861=EDGE_CURVE('',#2378,#2378,#2031,.T.);
#2862=EDGE_CURVE('',#2378,#2379,#1519,.T.);
#2863=EDGE_CURVE('',#2379,#2379,#2032,.T.);
#2864=EDGE_CURVE('',#2380,#2380,#2033,.T.);
#2865=EDGE_CURVE('',#2380,#2381,#1520,.T.);
#2866=EDGE_CURVE('',#2381,#2381,#2034,.T.);
#2867=EDGE_CURVE('',#2382,#2382,#2035,.T.);
#2868=EDGE_CURVE('',#2382,#2383,#1521,.T.);
#2869=EDGE_CURVE('',#2383,#2383,#2036,.T.);
#2870=EDGE_CURVE('',#2384,#2384,#2037,.T.);
#2871=EDGE_CURVE('',#2384,#2385,#1522,.T.);
#2872=EDGE_CURVE('',#2385,#2385,#2038,.T.);
#2873=EDGE_CURVE('',#2386,#2386,#2039,.T.);
#2874=EDGE_CURVE('',#2386,#2387,#1523,.T.);
#2875=EDGE_CURVE('',#2387,#2387,#2040,.T.);
#2876=EDGE_CURVE('',#2388,#2388,#2041,.T.);
#2877=EDGE_CURVE('',#2388,#2389,#1524,.T.);
#2878=EDGE_CURVE('',#2389,#2389,#2042,.T.);
#2879=EDGE_CURVE('',#2390,#2390,#2043,.T.);
#2880=EDGE_CURVE('',#2390,#2391,#1525,.T.);
#2881=EDGE_CURVE('',#2391,#2391,#2044,.T.);
#2882=EDGE_CURVE('',#2392,#2392,#2045,.T.);
#2883=EDGE_CURVE('',#2392,#2393,#1526,.T.);
#2884=EDGE_CURVE('',#2393,#2393,#2046,.T.);
#2885=EDGE_CURVE('',#2394,#2394,#2047,.T.);
#2886=EDGE_CURVE('',#2395,#2395,#2048,.T.);
#2887=EDGE_CURVE('',#2395,#2396,#1527,.T.);
#2888=EDGE_CURVE('',#2396,#2396,#2049,.T.);
#2889=EDGE_CURVE('',#2397,#2397,#2050,.T.);
#2890=EDGE_CURVE('',#2398,#2398,#2051,.T.);
#2891=EDGE_CURVE('',#2399,#2399,#2052,.T.);
#2892=EDGE_CURVE('',#2400,#2400,#2053,.T.);
#2893=EDGE_CURVE('',#2400,#2394,#1528,.T.);
#2894=EDGE_CURVE('',#2401,#2401,#2054,.T.);
#2895=EDGE_CURVE('',#2401,#2398,#1529,.T.);
#2896=EDGE_CURVE('',#2397,#2402,#1530,.T.);
#2897=EDGE_CURVE('',#2402,#2402,#2055,.T.);
#2898=EDGE_CURVE('',#2399,#2403,#1531,.T.);
#2899=EDGE_CURVE('',#2403,#2403,#2056,.T.);
#2900=EDGE_CURVE('',#2404,#2404,#2057,.T.);
#2901=EDGE_CURVE('',#2404,#2405,#1532,.T.);
#2902=EDGE_CURVE('',#2405,#2405,#2058,.T.);
#2903=EDGE_CURVE('',#2406,#2406,#2059,.T.);
#2904=EDGE_CURVE('',#2406,#2407,#1533,.T.);
#2905=EDGE_CURVE('',#2407,#2407,#2060,.T.);
#2906=EDGE_CURVE('',#2408,#2408,#2061,.T.);
#2907=EDGE_CURVE('',#2408,#2409,#1534,.T.);
#2908=EDGE_CURVE('',#2409,#2409,#2062,.T.);
#2909=EDGE_CURVE('',#2410,#2410,#2063,.T.);
#2910=EDGE_CURVE('',#2410,#2411,#1535,.T.);
#2911=EDGE_CURVE('',#2411,#2411,#2064,.T.);
#2912=EDGE_CURVE('',#2412,#2412,#2065,.T.);
#2913=EDGE_CURVE('',#2412,#2413,#1536,.T.);
#2914=EDGE_CURVE('',#2413,#2413,#2066,.T.);
#2915=EDGE_CURVE('',#2414,#2414,#2067,.T.);
#2916=EDGE_CURVE('',#2414,#2415,#1537,.T.);
#2917=EDGE_CURVE('',#2415,#2415,#2068,.T.);
#2918=EDGE_CURVE('',#2416,#2416,#2069,.T.);
#2919=EDGE_CURVE('',#2416,#2417,#1538,.T.);
#2920=EDGE_CURVE('',#2417,#2417,#2070,.T.);
#2921=EDGE_CURVE('',#2418,#2418,#2071,.T.);
#2922=EDGE_CURVE('',#2418,#2419,#1539,.T.);
#2923=EDGE_CURVE('',#2419,#2419,#2072,.T.);
#2924=EDGE_CURVE('',#2420,#2420,#2073,.T.);
#2925=EDGE_CURVE('',#2420,#2421,#1540,.T.);
#2926=EDGE_CURVE('',#2421,#2421,#2074,.T.);
#2927=EDGE_CURVE('',#2422,#2422,#2075,.T.);
#2928=EDGE_CURVE('',#2422,#2423,#1541,.T.);
#2929=EDGE_CURVE('',#2423,#2423,#2076,.T.);
#2930=EDGE_CURVE('',#2424,#2424,#2077,.T.);
#2931=EDGE_CURVE('',#2424,#2425,#1542,.T.);
#2932=EDGE_CURVE('',#2425,#2425,#2078,.T.);
#2933=EDGE_CURVE('',#2426,#2426,#2079,.T.);
#2934=EDGE_CURVE('',#2426,#2427,#1543,.T.);
#2935=EDGE_CURVE('',#2427,#2427,#2080,.T.);
#2936=EDGE_CURVE('',#2428,#2428,#2081,.T.);
#2937=EDGE_CURVE('',#2428,#2429,#1544,.T.);
#2938=EDGE_CURVE('',#2429,#2429,#2082,.T.);
#2939=EDGE_CURVE('',#2430,#2430,#2083,.T.);
#2940=EDGE_CURVE('',#2430,#2431,#1545,.T.);
#2941=EDGE_CURVE('',#2431,#2431,#2084,.T.);
#2942=EDGE_CURVE('',#2432,#2432,#2085,.T.);
#2943=EDGE_CURVE('',#2432,#2433,#1546,.T.);
#2944=EDGE_CURVE('',#2433,#2433,#2086,.T.);
#2945=EDGE_CURVE('',#2434,#2434,#2087,.T.);
#2946=EDGE_CURVE('',#2434,#2435,#1547,.T.);
#2947=EDGE_CURVE('',#2435,#2435,#2088,.T.);
#2948=EDGE_CURVE('',#2436,#2436,#2089,.T.);
#2949=EDGE_CURVE('',#2436,#2437,#1548,.T.);
#2950=EDGE_CURVE('',#2437,#2437,#2090,.T.);
#2951=EDGE_CURVE('',#2438,#2438,#2091,.T.);
#2952=EDGE_CURVE('',#2438,#2439,#1549,.T.);
#2953=EDGE_CURVE('',#2439,#2439,#2092,.T.);
#2954=EDGE_CURVE('',#2440,#2440,#2093,.T.);
#2955=EDGE_CURVE('',#2440,#2441,#1550,.T.);
#2956=EDGE_CURVE('',#2441,#2441,#2094,.T.);
#2957=EDGE_CURVE('',#2442,#2442,#2095,.T.);
#2958=EDGE_CURVE('',#2442,#2443,#1551,.T.);
#2959=EDGE_CURVE('',#2443,#2443,#2096,.T.);
#2960=EDGE_CURVE('',#2444,#2444,#2097,.T.);
#2961=EDGE_CURVE('',#2444,#2445,#1552,.T.);
#2962=EDGE_CURVE('',#2445,#2445,#2098,.T.);
#2963=EDGE_CURVE('',#2446,#2446,#2099,.T.);
#2964=EDGE_CURVE('',#2446,#2447,#1553,.T.);
#2965=EDGE_CURVE('',#2447,#2447,#2100,.T.);
#2966=EDGE_CURVE('',#2448,#2448,#2101,.T.);
#2967=EDGE_CURVE('',#2448,#2449,#1554,.T.);
#2968=EDGE_CURVE('',#2449,#2449,#2102,.T.);
#2969=EDGE_CURVE('',#2450,#2450,#2103,.T.);
#2970=EDGE_CURVE('',#2450,#2451,#1555,.T.);
#2971=EDGE_CURVE('',#2451,#2451,#2104,.T.);
#2972=EDGE_CURVE('',#2452,#2452,#2105,.T.);
#2973=EDGE_CURVE('',#2452,#2453,#1556,.T.);
#2974=EDGE_CURVE('',#2453,#2453,#2106,.T.);
#2975=EDGE_CURVE('',#2454,#2454,#2107,.T.);
#2976=EDGE_CURVE('',#2454,#2455,#1557,.T.);
#2977=EDGE_CURVE('',#2455,#2455,#2108,.T.);
#2978=EDGE_CURVE('',#2456,#2456,#2109,.T.);
#2979=EDGE_CURVE('',#2456,#2457,#1558,.T.);
#2980=EDGE_CURVE('',#2457,#2457,#2110,.T.);
#2981=EDGE_CURVE('',#2458,#2458,#2111,.T.);
#2982=EDGE_CURVE('',#2459,#2459,#2112,.T.);
#2983=EDGE_CURVE('',#2459,#2458,#1559,.T.);
#2984=EDGE_CURVE('',#2460,#2460,#2113,.T.);
#2985=EDGE_CURVE('',#2460,#2459,#1560,.T.);
#2986=EDGE_CURVE('',#2461,#2461,#2114,.T.);
#2987=EDGE_CURVE('',#2461,#2460,#1561,.T.);
#2988=EDGE_CURVE('',#2462,#2462,#2115,.T.);
#2989=EDGE_CURVE('',#2463,#2463,#2116,.F.);
#2990=EDGE_CURVE('',#2463,#2462,#1562,.T.);
#2991=EDGE_CURVE('',#2464,#2464,#2117,.F.);
#2992=EDGE_CURVE('',#2464,#2463,#1563,.T.);
#2993=EDGE_CURVE('',#2465,#2465,#2118,.T.);
#2994=EDGE_CURVE('',#2465,#2464,#1564,.T.);
#2995=EDGE_CURVE('',#2466,#2467,#1565,.T.);
#2996=EDGE_CURVE('',#2467,#2468,#1566,.T.);
#2997=EDGE_CURVE('',#2468,#2469,#1567,.T.);
#2998=EDGE_CURVE('',#2466,#2469,#1568,.T.);
#2999=EDGE_CURVE('',#2467,#2470,#1569,.T.);
#3000=EDGE_CURVE('',#2470,#2471,#1570,.T.);
#3001=EDGE_CURVE('',#2471,#2468,#1571,.T.);
#3002=EDGE_CURVE('',#2470,#2472,#1572,.T.);
#3003=EDGE_CURVE('',#2472,#2473,#1573,.T.);
#3004=EDGE_CURVE('',#2473,#2471,#1574,.T.);
#3005=EDGE_CURVE('',#2472,#2474,#1575,.T.);
#3006=EDGE_CURVE('',#2474,#2475,#1576,.T.);
#3007=EDGE_CURVE('',#2475,#2473,#1577,.T.);
#3008=EDGE_CURVE('',#2474,#2476,#1578,.T.);
#3009=EDGE_CURVE('',#2476,#2477,#1579,.T.);
#3010=EDGE_CURVE('',#2477,#2475,#1580,.T.);
#3011=EDGE_CURVE('',#2476,#2466,#1581,.T.);
#3012=EDGE_CURVE('',#2469,#2477,#1582,.T.);
#3013=EDGE_CURVE('',#2478,#2478,#2119,.T.);
#3014=EDGE_CURVE('',#2479,#2479,#2120,.T.);
#3015=EDGE_CURVE('',#2480,#2480,#2121,.T.);
#3016=EDGE_CURVE('',#2481,#2481,#2122,.T.);
#3017=EDGE_CURVE('',#2482,#2482,#2123,.T.);
#3018=EDGE_CURVE('',#2479,#2481,#1583,.T.);
#3019=EDGE_CURVE('',#2482,#2478,#1584,.T.);
#3020=EDGE_CURVE('',#2483,#2483,#2124,.T.);
#3021=EDGE_CURVE('',#2483,#2480,#1585,.T.);
#3022=EDGE_CURVE('',#2484,#2485,#1586,.T.);
#3023=EDGE_CURVE('',#2484,#2485,#2125,.T.);
#3024=EDGE_CURVE('',#2486,#2484,#258,.T.);
#3025=EDGE_CURVE('',#2487,#2486,#2126,.T.);
#3026=EDGE_CURVE('',#2488,#2487,#259,.T.);
#3027=EDGE_CURVE('',#2488,#2489,#1587,.T.);
#3028=EDGE_CURVE('',#2490,#2489,#260,.T.);
#3029=EDGE_CURVE('',#2489,#2490,#261,.T.);
#3030=EDGE_CURVE('',#2485,#2488,#262,.T.);
#3031=EDGE_CURVE('',#2487,#2486,#1588,.T.);
#3032=EDGE_CURVE('',#2491,#2491,#2127,.T.);
#3033=EDGE_CURVE('',#2491,#2492,#1589,.T.);
#3034=EDGE_CURVE('',#2492,#2492,#2128,.T.);
#3035=EDGE_CURVE('',#2493,#2493,#2129,.T.);
#3036=EDGE_CURVE('',#2493,#2494,#1590,.T.);
#3037=EDGE_CURVE('',#2494,#2494,#2130,.T.);
#3038=EDGE_CURVE('',#2495,#2496,#1591,.T.);
#3039=EDGE_CURVE('',#2495,#2497,#1592,.T.);
#3040=EDGE_CURVE('',#2497,#2498,#1593,.T.);
#3041=EDGE_CURVE('',#2496,#2498,#1594,.T.);
#3042=EDGE_CURVE('',#2499,#2495,#1595,.T.);
#3043=EDGE_CURVE('',#2499,#2500,#1596,.T.);
#3044=EDGE_CURVE('',#2500,#2497,#1597,.T.);
#3045=EDGE_CURVE('',#2501,#2499,#1598,.T.);
#3046=EDGE_CURVE('',#2501,#2502,#1599,.T.);
#3047=EDGE_CURVE('',#2502,#2500,#1600,.T.);
#3048=EDGE_CURVE('',#2503,#2501,#1601,.T.);
#3049=EDGE_CURVE('',#2503,#2504,#1602,.T.);
#3050=EDGE_CURVE('',#2504,#2502,#1603,.T.);
#3051=EDGE_CURVE('',#2505,#2503,#1604,.T.);
#3052=EDGE_CURVE('',#2505,#2506,#1605,.T.);
#3053=EDGE_CURVE('',#2506,#2504,#1606,.T.);
#3054=EDGE_CURVE('',#2496,#2505,#1607,.T.);
#3055=EDGE_CURVE('',#2498,#2506,#1608,.T.);
#3056=EDGE_CURVE('',#2507,#2507,#2131,.T.);
#3057=EDGE_CURVE('',#2508,#2508,#2132,.T.);
#3058=EDGE_CURVE('',#2508,#2507,#1609,.T.);
#3059=EDGE_CURVE('',#2509,#2509,#2133,.F.);
#3060=EDGE_CURVE('',#2509,#2508,#1610,.T.);
#3061=EDGE_CURVE('',#2510,#2510,#2134,.T.);
#3062=EDGE_CURVE('',#2510,#2509,#1611,.T.);
#3063=ORIENTED_EDGE('',*,*,#2511,.F.);
#3064=ORIENTED_EDGE('',*,*,#2512,.T.);
#3065=ORIENTED_EDGE('',*,*,#2513,.F.);
#3066=ORIENTED_EDGE('',*,*,#2512,.F.);
#3067=ORIENTED_EDGE('',*,*,#2514,.F.);
#3068=ORIENTED_EDGE('',*,*,#2515,.T.);
#3069=ORIENTED_EDGE('',*,*,#2516,.F.);
#3070=ORIENTED_EDGE('',*,*,#2515,.F.);
#3071=ORIENTED_EDGE('',*,*,#2517,.F.);
#3072=ORIENTED_EDGE('',*,*,#2518,.T.);
#3073=ORIENTED_EDGE('',*,*,#2519,.F.);
#3074=ORIENTED_EDGE('',*,*,#2518,.F.);
#3075=ORIENTED_EDGE('',*,*,#2520,.F.);
#3076=ORIENTED_EDGE('',*,*,#2521,.T.);
#3077=ORIENTED_EDGE('',*,*,#2522,.F.);
#3078=ORIENTED_EDGE('',*,*,#2521,.F.);
#3079=ORIENTED_EDGE('',*,*,#2523,.F.);
#3080=ORIENTED_EDGE('',*,*,#2524,.T.);
#3081=ORIENTED_EDGE('',*,*,#2525,.F.);
#3082=ORIENTED_EDGE('',*,*,#2524,.F.);
#3083=ORIENTED_EDGE('',*,*,#2526,.F.);
#3084=ORIENTED_EDGE('',*,*,#2527,.T.);
#3085=ORIENTED_EDGE('',*,*,#2528,.F.);
#3086=ORIENTED_EDGE('',*,*,#2527,.F.);
#3087=ORIENTED_EDGE('',*,*,#2529,.F.);
#3088=ORIENTED_EDGE('',*,*,#2530,.T.);
#3089=ORIENTED_EDGE('',*,*,#2531,.F.);
#3090=ORIENTED_EDGE('',*,*,#2530,.F.);
#3091=ORIENTED_EDGE('',*,*,#2532,.T.);
#3092=ORIENTED_EDGE('',*,*,#2533,.T.);
#3093=ORIENTED_EDGE('',*,*,#2534,.F.);
#3094=ORIENTED_EDGE('',*,*,#2535,.F.);
#3095=ORIENTED_EDGE('',*,*,#2536,.T.);
#3096=ORIENTED_EDGE('',*,*,#2535,.T.);
#3097=ORIENTED_EDGE('',*,*,#2537,.F.);
#3098=ORIENTED_EDGE('',*,*,#2538,.F.);
#3099=ORIENTED_EDGE('',*,*,#2539,.T.);
#3100=ORIENTED_EDGE('',*,*,#2538,.T.);
#3101=ORIENTED_EDGE('',*,*,#2540,.F.);
#3102=ORIENTED_EDGE('',*,*,#2541,.F.);
#3103=ORIENTED_EDGE('',*,*,#2542,.T.);
#3104=ORIENTED_EDGE('',*,*,#2541,.T.);
#3105=ORIENTED_EDGE('',*,*,#2543,.F.);
#3106=ORIENTED_EDGE('',*,*,#2533,.F.);
#3107=ORIENTED_EDGE('',*,*,#2543,.T.);
#3108=ORIENTED_EDGE('',*,*,#2540,.T.);
#3109=ORIENTED_EDGE('',*,*,#2537,.T.);
#3110=ORIENTED_EDGE('',*,*,#2534,.T.);
#3111=ORIENTED_EDGE('',*,*,#2531,.T.);
#3112=ORIENTED_EDGE('',*,*,#2528,.T.);
#3113=ORIENTED_EDGE('',*,*,#2525,.T.);
#3114=ORIENTED_EDGE('',*,*,#2522,.T.);
#3115=ORIENTED_EDGE('',*,*,#2519,.T.);
#3116=ORIENTED_EDGE('',*,*,#2516,.T.);
#3117=ORIENTED_EDGE('',*,*,#2513,.T.);
#3118=ORIENTED_EDGE('',*,*,#2542,.F.);
#3119=ORIENTED_EDGE('',*,*,#2532,.F.);
#3120=ORIENTED_EDGE('',*,*,#2536,.F.);
#3121=ORIENTED_EDGE('',*,*,#2539,.F.);
#3122=ORIENTED_EDGE('',*,*,#2529,.T.);
#3123=ORIENTED_EDGE('',*,*,#2526,.T.);
#3124=ORIENTED_EDGE('',*,*,#2523,.T.);
#3125=ORIENTED_EDGE('',*,*,#2520,.T.);
#3126=ORIENTED_EDGE('',*,*,#2517,.T.);
#3127=ORIENTED_EDGE('',*,*,#2514,.T.);
#3128=ORIENTED_EDGE('',*,*,#2511,.T.);
#3129=ORIENTED_EDGE('',*,*,#2544,.F.);
#3130=ORIENTED_EDGE('',*,*,#2545,.T.);
#3131=ORIENTED_EDGE('',*,*,#2546,.T.);
#3132=ORIENTED_EDGE('',*,*,#2545,.F.);
#3133=ORIENTED_EDGE('',*,*,#2544,.T.);
#3134=ORIENTED_EDGE('',*,*,#2546,.F.);
#3135=ORIENTED_EDGE('',*,*,#2547,.F.);
#3136=ORIENTED_EDGE('',*,*,#2548,.T.);
#3137=ORIENTED_EDGE('',*,*,#2549,.T.);
#3138=ORIENTED_EDGE('',*,*,#2548,.F.);
#3139=ORIENTED_EDGE('',*,*,#2547,.T.);
#3140=ORIENTED_EDGE('',*,*,#2549,.F.);
#3141=ORIENTED_EDGE('',*,*,#2550,.F.);
#3142=ORIENTED_EDGE('',*,*,#2551,.T.);
#3143=ORIENTED_EDGE('',*,*,#2552,.T.);
#3144=ORIENTED_EDGE('',*,*,#2551,.F.);
#3145=ORIENTED_EDGE('',*,*,#2550,.T.);
#3146=ORIENTED_EDGE('',*,*,#2552,.F.);
#3147=ORIENTED_EDGE('',*,*,#2553,.F.);
#3148=ORIENTED_EDGE('',*,*,#2554,.T.);
#3149=ORIENTED_EDGE('',*,*,#2555,.T.);
#3150=ORIENTED_EDGE('',*,*,#2554,.F.);
#3151=ORIENTED_EDGE('',*,*,#2553,.T.);
#3152=ORIENTED_EDGE('',*,*,#2555,.F.);
#3153=ORIENTED_EDGE('',*,*,#2556,.F.);
#3154=ORIENTED_EDGE('',*,*,#2557,.T.);
#3155=ORIENTED_EDGE('',*,*,#2558,.F.);
#3156=ORIENTED_EDGE('',*,*,#2557,.F.);
#3157=ORIENTED_EDGE('',*,*,#2559,.F.);
#3158=ORIENTED_EDGE('',*,*,#2560,.T.);
#3159=ORIENTED_EDGE('',*,*,#2561,.F.);
#3160=ORIENTED_EDGE('',*,*,#2560,.F.);
#3161=ORIENTED_EDGE('',*,*,#2562,.F.);
#3162=ORIENTED_EDGE('',*,*,#2563,.T.);
#3163=ORIENTED_EDGE('',*,*,#2564,.F.);
#3164=ORIENTED_EDGE('',*,*,#2563,.F.);
#3165=ORIENTED_EDGE('',*,*,#2565,.F.);
#3166=ORIENTED_EDGE('',*,*,#2566,.T.);
#3167=ORIENTED_EDGE('',*,*,#2567,.F.);
#3168=ORIENTED_EDGE('',*,*,#2566,.F.);
#3169=ORIENTED_EDGE('',*,*,#2568,.T.);
#3170=ORIENTED_EDGE('',*,*,#2569,.F.);
#3171=ORIENTED_EDGE('',*,*,#2570,.F.);
#3172=ORIENTED_EDGE('',*,*,#2571,.F.);
#3173=ORIENTED_EDGE('',*,*,#2568,.F.);
#3174=ORIENTED_EDGE('',*,*,#2572,.T.);
#3175=ORIENTED_EDGE('',*,*,#2570,.T.);
#3176=ORIENTED_EDGE('',*,*,#2572,.F.);
#3177=ORIENTED_EDGE('',*,*,#2571,.T.);
#3178=ORIENTED_EDGE('',*,*,#2573,.T.);
#3179=ORIENTED_EDGE('',*,*,#2574,.T.);
#3180=ORIENTED_EDGE('',*,*,#2573,.F.);
#3181=ORIENTED_EDGE('',*,*,#2575,.T.);
#3182=ORIENTED_EDGE('',*,*,#2574,.F.);
#3183=ORIENTED_EDGE('',*,*,#2567,.T.);
#3184=ORIENTED_EDGE('',*,*,#2564,.T.);
#3185=ORIENTED_EDGE('',*,*,#2561,.T.);
#3186=ORIENTED_EDGE('',*,*,#2558,.T.);
#3187=ORIENTED_EDGE('',*,*,#2575,.F.);
#3188=ORIENTED_EDGE('',*,*,#2576,.T.);
#3189=ORIENTED_EDGE('',*,*,#2577,.T.);
#3190=ORIENTED_EDGE('',*,*,#2576,.F.);
#3191=ORIENTED_EDGE('',*,*,#2578,.F.);
#3192=ORIENTED_EDGE('',*,*,#2579,.T.);
#3193=ORIENTED_EDGE('',*,*,#2569,.T.);
#3194=ORIENTED_EDGE('',*,*,#2579,.F.);
#3195=ORIENTED_EDGE('',*,*,#2578,.T.);
#3196=ORIENTED_EDGE('',*,*,#2577,.F.);
#3197=ORIENTED_EDGE('',*,*,#2556,.T.);
#3198=ORIENTED_EDGE('',*,*,#2559,.T.);
#3199=ORIENTED_EDGE('',*,*,#2562,.T.);
#3200=ORIENTED_EDGE('',*,*,#2565,.T.);
#3201=ORIENTED_EDGE('',*,*,#2580,.F.);
#3202=ORIENTED_EDGE('',*,*,#2581,.T.);
#3203=ORIENTED_EDGE('',*,*,#2582,.T.);
#3204=ORIENTED_EDGE('',*,*,#2581,.F.);
#3205=ORIENTED_EDGE('',*,*,#2583,.F.);
#3206=ORIENTED_EDGE('',*,*,#2584,.T.);
#3207=ORIENTED_EDGE('',*,*,#2585,.T.);
#3208=ORIENTED_EDGE('',*,*,#2584,.F.);
#3209=ORIENTED_EDGE('',*,*,#2583,.T.);
#3210=ORIENTED_EDGE('',*,*,#2580,.T.);
#3211=ORIENTED_EDGE('',*,*,#2585,.F.);
#3212=ORIENTED_EDGE('',*,*,#2582,.F.);
#3213=ORIENTED_EDGE('',*,*,#2586,.F.);
#3214=ORIENTED_EDGE('',*,*,#2587,.T.);
#3215=ORIENTED_EDGE('',*,*,#2588,.F.);
#3216=ORIENTED_EDGE('',*,*,#2589,.F.);
#3217=ORIENTED_EDGE('',*,*,#2590,.F.);
#3218=ORIENTED_EDGE('',*,*,#2591,.T.);
#3219=ORIENTED_EDGE('',*,*,#2592,.F.);
#3220=ORIENTED_EDGE('',*,*,#2593,.F.);
#3221=ORIENTED_EDGE('',*,*,#2591,.F.);
#3222=ORIENTED_EDGE('',*,*,#2594,.F.);
#3223=ORIENTED_EDGE('',*,*,#2587,.F.);
#3224=ORIENTED_EDGE('',*,*,#2595,.F.);
#3225=ORIENTED_EDGE('',*,*,#2589,.T.);
#3226=ORIENTED_EDGE('',*,*,#2596,.F.);
#3227=ORIENTED_EDGE('',*,*,#2597,.T.);
#3228=ORIENTED_EDGE('',*,*,#2598,.T.);
#3229=ORIENTED_EDGE('',*,*,#2597,.F.);
#3230=ORIENTED_EDGE('',*,*,#2594,.T.);
#3231=ORIENTED_EDGE('',*,*,#2590,.T.);
#3232=ORIENTED_EDGE('',*,*,#2595,.T.);
#3233=ORIENTED_EDGE('',*,*,#2588,.T.);
#3234=ORIENTED_EDGE('',*,*,#2586,.T.);
#3235=ORIENTED_EDGE('',*,*,#2599,.F.);
#3236=ORIENTED_EDGE('',*,*,#2600,.T.);
#3237=ORIENTED_EDGE('',*,*,#2601,.T.);
#3238=ORIENTED_EDGE('',*,*,#2600,.F.);
#3239=ORIENTED_EDGE('',*,*,#2592,.T.);
#3240=ORIENTED_EDGE('',*,*,#2593,.T.);
#3241=ORIENTED_EDGE('',*,*,#2599,.T.);
#3242=ORIENTED_EDGE('',*,*,#2596,.T.);
#3243=ORIENTED_EDGE('',*,*,#2601,.F.);
#3244=ORIENTED_EDGE('',*,*,#2598,.F.);
#3245=ORIENTED_EDGE('',*,*,#2602,.F.);
#3246=ORIENTED_EDGE('',*,*,#2603,.T.);
#3247=ORIENTED_EDGE('',*,*,#2604,.F.);
#3248=ORIENTED_EDGE('',*,*,#2603,.F.);
#3249=ORIENTED_EDGE('',*,*,#2605,.F.);
#3250=ORIENTED_EDGE('',*,*,#2606,.T.);
#3251=ORIENTED_EDGE('',*,*,#2607,.F.);
#3252=ORIENTED_EDGE('',*,*,#2606,.F.);
#3253=ORIENTED_EDGE('',*,*,#2608,.F.);
#3254=ORIENTED_EDGE('',*,*,#2609,.T.);
#3255=ORIENTED_EDGE('',*,*,#2610,.F.);
#3256=ORIENTED_EDGE('',*,*,#2609,.F.);
#3257=ORIENTED_EDGE('',*,*,#2608,.T.);
#3258=ORIENTED_EDGE('',*,*,#2611,.F.);
#3259=ORIENTED_EDGE('',*,*,#2611,.T.);
#3260=ORIENTED_EDGE('',*,*,#2612,.T.);
#3261=ORIENTED_EDGE('',*,*,#2613,.T.);
#3262=ORIENTED_EDGE('',*,*,#2612,.F.);
#3263=ORIENTED_EDGE('',*,*,#2614,.F.);
#3264=ORIENTED_EDGE('',*,*,#2615,.T.);
#3265=ORIENTED_EDGE('',*,*,#2616,.T.);
#3266=ORIENTED_EDGE('',*,*,#2615,.F.);
#3267=ORIENTED_EDGE('',*,*,#2614,.T.);
#3268=ORIENTED_EDGE('',*,*,#2604,.T.);
#3269=ORIENTED_EDGE('',*,*,#2607,.T.);
#3270=ORIENTED_EDGE('',*,*,#2610,.T.);
#3271=ORIENTED_EDGE('',*,*,#2616,.F.);
#3272=ORIENTED_EDGE('',*,*,#2602,.T.);
#3273=ORIENTED_EDGE('',*,*,#2605,.T.);
#3274=ORIENTED_EDGE('',*,*,#2613,.F.);
#3275=ORIENTED_EDGE('',*,*,#2617,.F.);
#3276=ORIENTED_EDGE('',*,*,#2618,.T.);
#3277=ORIENTED_EDGE('',*,*,#2619,.T.);
#3278=ORIENTED_EDGE('',*,*,#2618,.F.);
#3279=ORIENTED_EDGE('',*,*,#2620,.F.);
#3280=ORIENTED_EDGE('',*,*,#2619,.F.);
#3281=ORIENTED_EDGE('',*,*,#2620,.T.);
#3282=ORIENTED_EDGE('',*,*,#2621,.T.);
#3283=ORIENTED_EDGE('',*,*,#2622,.T.);
#3284=ORIENTED_EDGE('',*,*,#2621,.F.);
#3285=ORIENTED_EDGE('',*,*,#2623,.F.);
#3286=ORIENTED_EDGE('',*,*,#2624,.T.);
#3287=ORIENTED_EDGE('',*,*,#2625,.T.);
#3288=ORIENTED_EDGE('',*,*,#2624,.F.);
#3289=ORIENTED_EDGE('',*,*,#2623,.T.);
#3290=ORIENTED_EDGE('',*,*,#2617,.T.);
#3291=ORIENTED_EDGE('',*,*,#2625,.F.);
#3292=ORIENTED_EDGE('',*,*,#2622,.F.);
#3293=ORIENTED_EDGE('',*,*,#2626,.T.);
#3294=ORIENTED_EDGE('',*,*,#2627,.T.);
#3295=ORIENTED_EDGE('',*,*,#2628,.F.);
#3296=ORIENTED_EDGE('',*,*,#2627,.F.);
#3297=ORIENTED_EDGE('',*,*,#2628,.T.);
#3298=ORIENTED_EDGE('',*,*,#2626,.F.);
#3299=ORIENTED_EDGE('',*,*,#2629,.F.);
#3300=ORIENTED_EDGE('',*,*,#2630,.T.);
#3301=ORIENTED_EDGE('',*,*,#2631,.T.);
#3302=ORIENTED_EDGE('',*,*,#2630,.F.);
#3303=ORIENTED_EDGE('',*,*,#2632,.F.);
#3304=ORIENTED_EDGE('',*,*,#2633,.T.);
#3305=ORIENTED_EDGE('',*,*,#2634,.T.);
#3306=ORIENTED_EDGE('',*,*,#2633,.F.);
#3307=ORIENTED_EDGE('',*,*,#2632,.T.);
#3308=ORIENTED_EDGE('',*,*,#2629,.T.);
#3309=ORIENTED_EDGE('',*,*,#2634,.F.);
#3310=ORIENTED_EDGE('',*,*,#2631,.F.);
#3311=ORIENTED_EDGE('',*,*,#2635,.T.);
#3312=ORIENTED_EDGE('',*,*,#2636,.T.);
#3313=ORIENTED_EDGE('',*,*,#2637,.T.);
#3314=ORIENTED_EDGE('',*,*,#2638,.F.);
#3315=ORIENTED_EDGE('',*,*,#2639,.T.);
#3316=ORIENTED_EDGE('',*,*,#2640,.T.);
#3317=ORIENTED_EDGE('',*,*,#2641,.T.);
#3318=ORIENTED_EDGE('',*,*,#2636,.F.);
#3319=ORIENTED_EDGE('',*,*,#2642,.T.);
#3320=ORIENTED_EDGE('',*,*,#2643,.T.);
#3321=ORIENTED_EDGE('',*,*,#2644,.T.);
#3322=ORIENTED_EDGE('',*,*,#2640,.F.);
#3323=ORIENTED_EDGE('',*,*,#2645,.T.);
#3324=ORIENTED_EDGE('',*,*,#2646,.T.);
#3325=ORIENTED_EDGE('',*,*,#2647,.T.);
#3326=ORIENTED_EDGE('',*,*,#2643,.F.);
#3327=ORIENTED_EDGE('',*,*,#2648,.T.);
#3328=ORIENTED_EDGE('',*,*,#2649,.T.);
#3329=ORIENTED_EDGE('',*,*,#2650,.T.);
#3330=ORIENTED_EDGE('',*,*,#2646,.F.);
#3331=ORIENTED_EDGE('',*,*,#2651,.T.);
#3332=ORIENTED_EDGE('',*,*,#2638,.T.);
#3333=ORIENTED_EDGE('',*,*,#2652,.T.);
#3334=ORIENTED_EDGE('',*,*,#2649,.F.);
#3335=ORIENTED_EDGE('',*,*,#2651,.F.);
#3336=ORIENTED_EDGE('',*,*,#2648,.F.);
#3337=ORIENTED_EDGE('',*,*,#2645,.F.);
#3338=ORIENTED_EDGE('',*,*,#2642,.F.);
#3339=ORIENTED_EDGE('',*,*,#2639,.F.);
#3340=ORIENTED_EDGE('',*,*,#2635,.F.);
#3341=ORIENTED_EDGE('',*,*,#2652,.F.);
#3342=ORIENTED_EDGE('',*,*,#2637,.F.);
#3343=ORIENTED_EDGE('',*,*,#2641,.F.);
#3344=ORIENTED_EDGE('',*,*,#2644,.F.);
#3345=ORIENTED_EDGE('',*,*,#2647,.F.);
#3346=ORIENTED_EDGE('',*,*,#2650,.F.);
#3347=ORIENTED_EDGE('',*,*,#2653,.F.);
#3348=ORIENTED_EDGE('',*,*,#2654,.F.);
#3349=ORIENTED_EDGE('',*,*,#2655,.F.);
#3350=ORIENTED_EDGE('',*,*,#2656,.T.);
#3351=ORIENTED_EDGE('',*,*,#2654,.T.);
#3352=ORIENTED_EDGE('',*,*,#2656,.F.);
#3353=ORIENTED_EDGE('',*,*,#2657,.F.);
#3354=ORIENTED_EDGE('',*,*,#2658,.T.);
#3355=ORIENTED_EDGE('',*,*,#2655,.T.);
#3356=ORIENTED_EDGE('',*,*,#2658,.F.);
#3357=ORIENTED_EDGE('',*,*,#2659,.F.);
#3358=ORIENTED_EDGE('',*,*,#2660,.T.);
#3359=ORIENTED_EDGE('',*,*,#2657,.T.);
#3360=ORIENTED_EDGE('',*,*,#2660,.F.);
#3361=ORIENTED_EDGE('',*,*,#2659,.T.);
#3362=ORIENTED_EDGE('',*,*,#2661,.F.);
#3363=ORIENTED_EDGE('',*,*,#2662,.F.);
#3364=ORIENTED_EDGE('',*,*,#2663,.T.);
#3365=ORIENTED_EDGE('',*,*,#2661,.T.);
#3366=ORIENTED_EDGE('',*,*,#2663,.F.);
#3367=ORIENTED_EDGE('',*,*,#2653,.T.);
#3368=ORIENTED_EDGE('',*,*,#2664,.T.);
#3369=ORIENTED_EDGE('',*,*,#2662,.T.);
#3370=ORIENTED_EDGE('',*,*,#2664,.F.);
#3371=ORIENTED_EDGE('',*,*,#2665,.F.);
#3372=ORIENTED_EDGE('',*,*,#2666,.F.);
#3373=ORIENTED_EDGE('',*,*,#2667,.T.);
#3374=ORIENTED_EDGE('',*,*,#2668,.F.);
#3375=ORIENTED_EDGE('',*,*,#2669,.F.);
#3376=ORIENTED_EDGE('',*,*,#2667,.F.);
#3377=ORIENTED_EDGE('',*,*,#2668,.T.);
#3378=ORIENTED_EDGE('',*,*,#2669,.T.);
#3379=ORIENTED_EDGE('',*,*,#2670,.T.);
#3380=ORIENTED_EDGE('',*,*,#2671,.T.);
#3381=ORIENTED_EDGE('',*,*,#2670,.F.);
#3382=ORIENTED_EDGE('',*,*,#2672,.T.);
#3383=ORIENTED_EDGE('',*,*,#2673,.T.);
#3384=ORIENTED_EDGE('',*,*,#2674,.F.);
#3385=ORIENTED_EDGE('',*,*,#2673,.F.);
#3386=ORIENTED_EDGE('',*,*,#2674,.T.);
#3387=ORIENTED_EDGE('',*,*,#2675,.T.);
#3388=ORIENTED_EDGE('',*,*,#2676,.F.);
#3389=ORIENTED_EDGE('',*,*,#2675,.F.);
#3390=ORIENTED_EDGE('',*,*,#2671,.F.);
#3391=ORIENTED_EDGE('',*,*,#2676,.T.);
#3392=ORIENTED_EDGE('',*,*,#2677,.F.);
#3393=ORIENTED_EDGE('',*,*,#2678,.T.);
#3394=ORIENTED_EDGE('',*,*,#2665,.T.);
#3395=ORIENTED_EDGE('',*,*,#2666,.T.);
#3396=ORIENTED_EDGE('',*,*,#2678,.F.);
#3397=ORIENTED_EDGE('',*,*,#2677,.T.);
#3398=ORIENTED_EDGE('',*,*,#2679,.F.);
#3399=ORIENTED_EDGE('',*,*,#2679,.T.);
#3400=ORIENTED_EDGE('',*,*,#2680,.T.);
#3401=ORIENTED_EDGE('',*,*,#2672,.F.);
#3402=ORIENTED_EDGE('',*,*,#2680,.F.);
#3403=ORIENTED_EDGE('',*,*,#2681,.F.);
#3404=ORIENTED_EDGE('',*,*,#2682,.F.);
#3405=ORIENTED_EDGE('',*,*,#2683,.T.);
#3406=ORIENTED_EDGE('',*,*,#2684,.F.);
#3407=ORIENTED_EDGE('',*,*,#2685,.F.);
#3408=ORIENTED_EDGE('',*,*,#2683,.F.);
#3409=ORIENTED_EDGE('',*,*,#2686,.T.);
#3410=ORIENTED_EDGE('',*,*,#2687,.T.);
#3411=ORIENTED_EDGE('',*,*,#2684,.T.);
#3412=ORIENTED_EDGE('',*,*,#2685,.T.);
#3413=ORIENTED_EDGE('',*,*,#2687,.F.);
#3414=ORIENTED_EDGE('',*,*,#2688,.F.);
#3415=ORIENTED_EDGE('',*,*,#2689,.T.);
#3416=ORIENTED_EDGE('',*,*,#2690,.F.);
#3417=ORIENTED_EDGE('',*,*,#2691,.T.);
#3418=ORIENTED_EDGE('',*,*,#2688,.T.);
#3419=ORIENTED_EDGE('',*,*,#2691,.F.);
#3420=ORIENTED_EDGE('',*,*,#2692,.F.);
#3421=ORIENTED_EDGE('',*,*,#2693,.T.);
#3422=ORIENTED_EDGE('',*,*,#2690,.T.);
#3423=ORIENTED_EDGE('',*,*,#2693,.F.);
#3424=ORIENTED_EDGE('',*,*,#2694,.F.);
#3425=ORIENTED_EDGE('',*,*,#2695,.T.);
#3426=ORIENTED_EDGE('',*,*,#2692,.T.);
#3427=ORIENTED_EDGE('',*,*,#2695,.F.);
#3428=ORIENTED_EDGE('',*,*,#2694,.T.);
#3429=ORIENTED_EDGE('',*,*,#2686,.F.);
#3430=ORIENTED_EDGE('',*,*,#2681,.T.);
#3431=ORIENTED_EDGE('',*,*,#2682,.T.);
#3432=ORIENTED_EDGE('',*,*,#2696,.T.);
#3433=ORIENTED_EDGE('',*,*,#2689,.F.);
#3434=ORIENTED_EDGE('',*,*,#2696,.F.);
#3435=ORIENTED_EDGE('',*,*,#2697,.T.);
#3436=ORIENTED_EDGE('',*,*,#2697,.F.);
#3437=ORIENTED_EDGE('',*,*,#2698,.T.);
#3438=ORIENTED_EDGE('',*,*,#2698,.F.);
#3439=ORIENTED_EDGE('',*,*,#2699,.T.);
#3440=ORIENTED_EDGE('',*,*,#2699,.F.);
#3441=ORIENTED_EDGE('',*,*,#2700,.T.);
#3442=ORIENTED_EDGE('',*,*,#2700,.F.);
#3443=ORIENTED_EDGE('',*,*,#2701,.T.);
#3444=ORIENTED_EDGE('',*,*,#2701,.F.);
#3445=ORIENTED_EDGE('',*,*,#2702,.T.);
#3446=ORIENTED_EDGE('',*,*,#2702,.F.);
#3447=ORIENTED_EDGE('',*,*,#2703,.T.);
#3448=ORIENTED_EDGE('',*,*,#2703,.F.);
#3449=ORIENTED_EDGE('',*,*,#2704,.T.);
#3450=ORIENTED_EDGE('',*,*,#2704,.F.);
#3451=ORIENTED_EDGE('',*,*,#2705,.T.);
#3452=ORIENTED_EDGE('',*,*,#2705,.F.);
#3453=ORIENTED_EDGE('',*,*,#2706,.F.);
#3454=ORIENTED_EDGE('',*,*,#2707,.F.);
#3455=ORIENTED_EDGE('',*,*,#2708,.F.);
#3456=ORIENTED_EDGE('',*,*,#2709,.F.);
#3457=ORIENTED_EDGE('',*,*,#2708,.T.);
#3458=ORIENTED_EDGE('',*,*,#2710,.F.);
#3459=ORIENTED_EDGE('',*,*,#2711,.T.);
#3460=ORIENTED_EDGE('',*,*,#2712,.F.);
#3461=ORIENTED_EDGE('',*,*,#2713,.T.);
#3462=ORIENTED_EDGE('',*,*,#2714,.F.);
#3463=ORIENTED_EDGE('',*,*,#2715,.T.);
#3464=ORIENTED_EDGE('',*,*,#2716,.F.);
#3465=ORIENTED_EDGE('',*,*,#2717,.T.);
#3466=ORIENTED_EDGE('',*,*,#2718,.F.);
#3467=ORIENTED_EDGE('',*,*,#2717,.F.);
#3468=ORIENTED_EDGE('',*,*,#2719,.F.);
#3469=ORIENTED_EDGE('',*,*,#2720,.T.);
#3470=ORIENTED_EDGE('',*,*,#2721,.F.);
#3471=ORIENTED_EDGE('',*,*,#2722,.T.);
#3472=ORIENTED_EDGE('',*,*,#2723,.F.);
#3473=ORIENTED_EDGE('',*,*,#2724,.T.);
#3474=ORIENTED_EDGE('',*,*,#2725,.F.);
#3475=ORIENTED_EDGE('',*,*,#2726,.T.);
#3476=ORIENTED_EDGE('',*,*,#2727,.F.);
#3477=ORIENTED_EDGE('',*,*,#2728,.T.);
#3478=ORIENTED_EDGE('',*,*,#2729,.F.);
#3479=ORIENTED_EDGE('',*,*,#2707,.T.);
#3480=ORIENTED_EDGE('',*,*,#2730,.T.);
#3481=ORIENTED_EDGE('',*,*,#2731,.T.);
#3482=ORIENTED_EDGE('',*,*,#2710,.T.);
#3483=ORIENTED_EDGE('',*,*,#2732,.F.);
#3484=ORIENTED_EDGE('',*,*,#2733,.F.);
#3485=ORIENTED_EDGE('',*,*,#2711,.F.);
#3486=ORIENTED_EDGE('',*,*,#2731,.F.);
#3487=ORIENTED_EDGE('',*,*,#2733,.T.);
#3488=ORIENTED_EDGE('',*,*,#2734,.T.);
#3489=ORIENTED_EDGE('',*,*,#2735,.T.);
#3490=ORIENTED_EDGE('',*,*,#2712,.T.);
#3491=ORIENTED_EDGE('',*,*,#2736,.F.);
#3492=ORIENTED_EDGE('',*,*,#2737,.F.);
#3493=ORIENTED_EDGE('',*,*,#2713,.F.);
#3494=ORIENTED_EDGE('',*,*,#2735,.F.);
#3495=ORIENTED_EDGE('',*,*,#2737,.T.);
#3496=ORIENTED_EDGE('',*,*,#2738,.T.);
#3497=ORIENTED_EDGE('',*,*,#2739,.T.);
#3498=ORIENTED_EDGE('',*,*,#2714,.T.);
#3499=ORIENTED_EDGE('',*,*,#2740,.F.);
#3500=ORIENTED_EDGE('',*,*,#2741,.F.);
#3501=ORIENTED_EDGE('',*,*,#2715,.F.);
#3502=ORIENTED_EDGE('',*,*,#2739,.F.);
#3503=ORIENTED_EDGE('',*,*,#2741,.T.);
#3504=ORIENTED_EDGE('',*,*,#2742,.T.);
#3505=ORIENTED_EDGE('',*,*,#2743,.T.);
#3506=ORIENTED_EDGE('',*,*,#2744,.T.);
#3507=ORIENTED_EDGE('',*,*,#2719,.T.);
#3508=ORIENTED_EDGE('',*,*,#2716,.T.);
#3509=ORIENTED_EDGE('',*,*,#2745,.F.);
#3510=ORIENTED_EDGE('',*,*,#2746,.F.);
#3511=ORIENTED_EDGE('',*,*,#2720,.F.);
#3512=ORIENTED_EDGE('',*,*,#2744,.F.);
#3513=ORIENTED_EDGE('',*,*,#2746,.T.);
#3514=ORIENTED_EDGE('',*,*,#2747,.T.);
#3515=ORIENTED_EDGE('',*,*,#2748,.T.);
#3516=ORIENTED_EDGE('',*,*,#2721,.T.);
#3517=ORIENTED_EDGE('',*,*,#2749,.F.);
#3518=ORIENTED_EDGE('',*,*,#2750,.F.);
#3519=ORIENTED_EDGE('',*,*,#2722,.F.);
#3520=ORIENTED_EDGE('',*,*,#2748,.F.);
#3521=ORIENTED_EDGE('',*,*,#2750,.T.);
#3522=ORIENTED_EDGE('',*,*,#2751,.T.);
#3523=ORIENTED_EDGE('',*,*,#2752,.T.);
#3524=ORIENTED_EDGE('',*,*,#2723,.T.);
#3525=ORIENTED_EDGE('',*,*,#2753,.F.);
#3526=ORIENTED_EDGE('',*,*,#2754,.F.);
#3527=ORIENTED_EDGE('',*,*,#2724,.F.);
#3528=ORIENTED_EDGE('',*,*,#2752,.F.);
#3529=ORIENTED_EDGE('',*,*,#2754,.T.);
#3530=ORIENTED_EDGE('',*,*,#2755,.T.);
#3531=ORIENTED_EDGE('',*,*,#2756,.T.);
#3532=ORIENTED_EDGE('',*,*,#2725,.T.);
#3533=ORIENTED_EDGE('',*,*,#2726,.F.);
#3534=ORIENTED_EDGE('',*,*,#2756,.F.);
#3535=ORIENTED_EDGE('',*,*,#2757,.F.);
#3536=ORIENTED_EDGE('',*,*,#2758,.F.);
#3537=ORIENTED_EDGE('',*,*,#2759,.F.);
#3538=ORIENTED_EDGE('',*,*,#2760,.T.);
#3539=ORIENTED_EDGE('',*,*,#2742,.F.);
#3540=ORIENTED_EDGE('',*,*,#2740,.T.);
#3541=ORIENTED_EDGE('',*,*,#2738,.F.);
#3542=ORIENTED_EDGE('',*,*,#2736,.T.);
#3543=ORIENTED_EDGE('',*,*,#2734,.F.);
#3544=ORIENTED_EDGE('',*,*,#2732,.T.);
#3545=ORIENTED_EDGE('',*,*,#2730,.F.);
#3546=ORIENTED_EDGE('',*,*,#2706,.T.);
#3547=ORIENTED_EDGE('',*,*,#2761,.F.);
#3548=ORIENTED_EDGE('',*,*,#2762,.T.);
#3549=ORIENTED_EDGE('',*,*,#2763,.F.);
#3550=ORIENTED_EDGE('',*,*,#2757,.T.);
#3551=ORIENTED_EDGE('',*,*,#2755,.F.);
#3552=ORIENTED_EDGE('',*,*,#2753,.T.);
#3553=ORIENTED_EDGE('',*,*,#2751,.F.);
#3554=ORIENTED_EDGE('',*,*,#2749,.T.);
#3555=ORIENTED_EDGE('',*,*,#2747,.F.);
#3556=ORIENTED_EDGE('',*,*,#2745,.T.);
#3557=ORIENTED_EDGE('',*,*,#2743,.F.);
#3558=ORIENTED_EDGE('',*,*,#2760,.F.);
#3559=ORIENTED_EDGE('',*,*,#2709,.T.);
#3560=ORIENTED_EDGE('',*,*,#2729,.T.);
#3561=ORIENTED_EDGE('',*,*,#2764,.T.);
#3562=ORIENTED_EDGE('',*,*,#2761,.T.);
#3563=ORIENTED_EDGE('',*,*,#2728,.F.);
#3564=ORIENTED_EDGE('',*,*,#2765,.F.);
#3565=ORIENTED_EDGE('',*,*,#2762,.F.);
#3566=ORIENTED_EDGE('',*,*,#2764,.F.);
#3567=ORIENTED_EDGE('',*,*,#2718,.T.);
#3568=ORIENTED_EDGE('',*,*,#2759,.T.);
#3569=ORIENTED_EDGE('',*,*,#2758,.T.);
#3570=ORIENTED_EDGE('',*,*,#2763,.T.);
#3571=ORIENTED_EDGE('',*,*,#2765,.T.);
#3572=ORIENTED_EDGE('',*,*,#2727,.T.);
#3573=ORIENTED_EDGE('',*,*,#2766,.F.);
#3574=ORIENTED_EDGE('',*,*,#2767,.T.);
#3575=ORIENTED_EDGE('',*,*,#2768,.F.);
#3576=ORIENTED_EDGE('',*,*,#2769,.T.);
#3577=ORIENTED_EDGE('',*,*,#2766,.T.);
#3578=ORIENTED_EDGE('',*,*,#2769,.F.);
#3579=ORIENTED_EDGE('',*,*,#2768,.T.);
#3580=ORIENTED_EDGE('',*,*,#2770,.F.);
#3581=ORIENTED_EDGE('',*,*,#2770,.T.);
#3582=ORIENTED_EDGE('',*,*,#2771,.T.);
#3583=ORIENTED_EDGE('',*,*,#2767,.F.);
#3584=ORIENTED_EDGE('',*,*,#2771,.F.);
#3585=ORIENTED_EDGE('',*,*,#2772,.F.);
#3586=ORIENTED_EDGE('',*,*,#2773,.T.);
#3587=ORIENTED_EDGE('',*,*,#2774,.F.);
#3588=ORIENTED_EDGE('',*,*,#2775,.T.);
#3589=ORIENTED_EDGE('',*,*,#2772,.T.);
#3590=ORIENTED_EDGE('',*,*,#2775,.F.);
#3591=ORIENTED_EDGE('',*,*,#2774,.T.);
#3592=ORIENTED_EDGE('',*,*,#2776,.F.);
#3593=ORIENTED_EDGE('',*,*,#2776,.T.);
#3594=ORIENTED_EDGE('',*,*,#2777,.T.);
#3595=ORIENTED_EDGE('',*,*,#2773,.F.);
#3596=ORIENTED_EDGE('',*,*,#2777,.F.);
#3597=ORIENTED_EDGE('',*,*,#2778,.F.);
#3598=ORIENTED_EDGE('',*,*,#2779,.F.);
#3599=ORIENTED_EDGE('',*,*,#2780,.T.);
#3600=ORIENTED_EDGE('',*,*,#2781,.T.);
#3601=ORIENTED_EDGE('',*,*,#2782,.F.);
#3602=ORIENTED_EDGE('',*,*,#2783,.F.);
#3603=ORIENTED_EDGE('',*,*,#2784,.T.);
#3604=ORIENTED_EDGE('',*,*,#2785,.T.);
#3605=ORIENTED_EDGE('',*,*,#2780,.F.);
#3606=ORIENTED_EDGE('',*,*,#2786,.F.);
#3607=ORIENTED_EDGE('',*,*,#2787,.T.);
#3608=ORIENTED_EDGE('',*,*,#2788,.T.);
#3609=ORIENTED_EDGE('',*,*,#2784,.F.);
#3610=ORIENTED_EDGE('',*,*,#2789,.F.);
#3611=ORIENTED_EDGE('',*,*,#2790,.T.);
#3612=ORIENTED_EDGE('',*,*,#2791,.T.);
#3613=ORIENTED_EDGE('',*,*,#2787,.F.);
#3614=ORIENTED_EDGE('',*,*,#2792,.F.);
#3615=ORIENTED_EDGE('',*,*,#2793,.T.);
#3616=ORIENTED_EDGE('',*,*,#2794,.T.);
#3617=ORIENTED_EDGE('',*,*,#2790,.F.);
#3618=ORIENTED_EDGE('',*,*,#2795,.F.);
#3619=ORIENTED_EDGE('',*,*,#2782,.T.);
#3620=ORIENTED_EDGE('',*,*,#2796,.T.);
#3621=ORIENTED_EDGE('',*,*,#2793,.F.);
#3622=ORIENTED_EDGE('',*,*,#2796,.F.);
#3623=ORIENTED_EDGE('',*,*,#2781,.F.);
#3624=ORIENTED_EDGE('',*,*,#2785,.F.);
#3625=ORIENTED_EDGE('',*,*,#2788,.F.);
#3626=ORIENTED_EDGE('',*,*,#2791,.F.);
#3627=ORIENTED_EDGE('',*,*,#2794,.F.);
#3628=ORIENTED_EDGE('',*,*,#2797,.F.);
#3629=ORIENTED_EDGE('',*,*,#2779,.T.);
#3630=ORIENTED_EDGE('',*,*,#2795,.T.);
#3631=ORIENTED_EDGE('',*,*,#2792,.T.);
#3632=ORIENTED_EDGE('',*,*,#2789,.T.);
#3633=ORIENTED_EDGE('',*,*,#2786,.T.);
#3634=ORIENTED_EDGE('',*,*,#2783,.T.);
#3635=ORIENTED_EDGE('',*,*,#2798,.F.);
#3636=ORIENTED_EDGE('',*,*,#2799,.T.);
#3637=ORIENTED_EDGE('',*,*,#2797,.T.);
#3638=ORIENTED_EDGE('',*,*,#2799,.F.);
#3639=ORIENTED_EDGE('',*,*,#2778,.T.);
#3640=ORIENTED_EDGE('',*,*,#2800,.T.);
#3641=ORIENTED_EDGE('',*,*,#2798,.T.);
#3642=ORIENTED_EDGE('',*,*,#2800,.F.);
#3643=ORIENTED_EDGE('',*,*,#2801,.F.);
#3644=ORIENTED_EDGE('',*,*,#2802,.T.);
#3645=ORIENTED_EDGE('',*,*,#2803,.T.);
#3646=ORIENTED_EDGE('',*,*,#2802,.F.);
#3647=ORIENTED_EDGE('',*,*,#2803,.F.);
#3648=ORIENTED_EDGE('',*,*,#2804,.F.);
#3649=ORIENTED_EDGE('',*,*,#2805,.T.);
#3650=ORIENTED_EDGE('',*,*,#2806,.T.);
#3651=ORIENTED_EDGE('',*,*,#2805,.F.);
#3652=ORIENTED_EDGE('',*,*,#2806,.F.);
#3653=ORIENTED_EDGE('',*,*,#2807,.F.);
#3654=ORIENTED_EDGE('',*,*,#2808,.T.);
#3655=ORIENTED_EDGE('',*,*,#2809,.T.);
#3656=ORIENTED_EDGE('',*,*,#2808,.F.);
#3657=ORIENTED_EDGE('',*,*,#2809,.F.);
#3658=ORIENTED_EDGE('',*,*,#2810,.F.);
#3659=ORIENTED_EDGE('',*,*,#2811,.T.);
#3660=ORIENTED_EDGE('',*,*,#2812,.T.);
#3661=ORIENTED_EDGE('',*,*,#2811,.F.);
#3662=ORIENTED_EDGE('',*,*,#2812,.F.);
#3663=ORIENTED_EDGE('',*,*,#2813,.F.);
#3664=ORIENTED_EDGE('',*,*,#2814,.T.);
#3665=ORIENTED_EDGE('',*,*,#2815,.T.);
#3666=ORIENTED_EDGE('',*,*,#2814,.F.);
#3667=ORIENTED_EDGE('',*,*,#2815,.F.);
#3668=ORIENTED_EDGE('',*,*,#2816,.F.);
#3669=ORIENTED_EDGE('',*,*,#2817,.T.);
#3670=ORIENTED_EDGE('',*,*,#2818,.T.);
#3671=ORIENTED_EDGE('',*,*,#2817,.F.);
#3672=ORIENTED_EDGE('',*,*,#2818,.F.);
#3673=ORIENTED_EDGE('',*,*,#2819,.F.);
#3674=ORIENTED_EDGE('',*,*,#2820,.T.);
#3675=ORIENTED_EDGE('',*,*,#2821,.T.);
#3676=ORIENTED_EDGE('',*,*,#2820,.F.);
#3677=ORIENTED_EDGE('',*,*,#2821,.F.);
#3678=ORIENTED_EDGE('',*,*,#2822,.F.);
#3679=ORIENTED_EDGE('',*,*,#2823,.T.);
#3680=ORIENTED_EDGE('',*,*,#2824,.T.);
#3681=ORIENTED_EDGE('',*,*,#2823,.F.);
#3682=ORIENTED_EDGE('',*,*,#2824,.F.);
#3683=ORIENTED_EDGE('',*,*,#2825,.F.);
#3684=ORIENTED_EDGE('',*,*,#2826,.T.);
#3685=ORIENTED_EDGE('',*,*,#2827,.T.);
#3686=ORIENTED_EDGE('',*,*,#2826,.F.);
#3687=ORIENTED_EDGE('',*,*,#2827,.F.);
#3688=ORIENTED_EDGE('',*,*,#2828,.F.);
#3689=ORIENTED_EDGE('',*,*,#2829,.T.);
#3690=ORIENTED_EDGE('',*,*,#2830,.T.);
#3691=ORIENTED_EDGE('',*,*,#2829,.F.);
#3692=ORIENTED_EDGE('',*,*,#2830,.F.);
#3693=ORIENTED_EDGE('',*,*,#2831,.F.);
#3694=ORIENTED_EDGE('',*,*,#2832,.T.);
#3695=ORIENTED_EDGE('',*,*,#2833,.T.);
#3696=ORIENTED_EDGE('',*,*,#2832,.F.);
#3697=ORIENTED_EDGE('',*,*,#2833,.F.);
#3698=ORIENTED_EDGE('',*,*,#2834,.F.);
#3699=ORIENTED_EDGE('',*,*,#2835,.T.);
#3700=ORIENTED_EDGE('',*,*,#2836,.T.);
#3701=ORIENTED_EDGE('',*,*,#2835,.F.);
#3702=ORIENTED_EDGE('',*,*,#2836,.F.);
#3703=ORIENTED_EDGE('',*,*,#2837,.F.);
#3704=ORIENTED_EDGE('',*,*,#2838,.T.);
#3705=ORIENTED_EDGE('',*,*,#2839,.T.);
#3706=ORIENTED_EDGE('',*,*,#2838,.F.);
#3707=ORIENTED_EDGE('',*,*,#2839,.F.);
#3708=ORIENTED_EDGE('',*,*,#2840,.F.);
#3709=ORIENTED_EDGE('',*,*,#2841,.T.);
#3710=ORIENTED_EDGE('',*,*,#2842,.T.);
#3711=ORIENTED_EDGE('',*,*,#2841,.F.);
#3712=ORIENTED_EDGE('',*,*,#2842,.F.);
#3713=ORIENTED_EDGE('',*,*,#2843,.F.);
#3714=ORIENTED_EDGE('',*,*,#2844,.T.);
#3715=ORIENTED_EDGE('',*,*,#2845,.T.);
#3716=ORIENTED_EDGE('',*,*,#2844,.F.);
#3717=ORIENTED_EDGE('',*,*,#2845,.F.);
#3718=ORIENTED_EDGE('',*,*,#2846,.F.);
#3719=ORIENTED_EDGE('',*,*,#2847,.T.);
#3720=ORIENTED_EDGE('',*,*,#2848,.T.);
#3721=ORIENTED_EDGE('',*,*,#2847,.F.);
#3722=ORIENTED_EDGE('',*,*,#2848,.F.);
#3723=ORIENTED_EDGE('',*,*,#2849,.F.);
#3724=ORIENTED_EDGE('',*,*,#2850,.T.);
#3725=ORIENTED_EDGE('',*,*,#2851,.T.);
#3726=ORIENTED_EDGE('',*,*,#2850,.F.);
#3727=ORIENTED_EDGE('',*,*,#2851,.F.);
#3728=ORIENTED_EDGE('',*,*,#2852,.F.);
#3729=ORIENTED_EDGE('',*,*,#2853,.T.);
#3730=ORIENTED_EDGE('',*,*,#2854,.T.);
#3731=ORIENTED_EDGE('',*,*,#2853,.F.);
#3732=ORIENTED_EDGE('',*,*,#2854,.F.);
#3733=ORIENTED_EDGE('',*,*,#2855,.F.);
#3734=ORIENTED_EDGE('',*,*,#2856,.T.);
#3735=ORIENTED_EDGE('',*,*,#2857,.T.);
#3736=ORIENTED_EDGE('',*,*,#2856,.F.);
#3737=ORIENTED_EDGE('',*,*,#2857,.F.);
#3738=ORIENTED_EDGE('',*,*,#2858,.F.);
#3739=ORIENTED_EDGE('',*,*,#2859,.T.);
#3740=ORIENTED_EDGE('',*,*,#2860,.T.);
#3741=ORIENTED_EDGE('',*,*,#2859,.F.);
#3742=ORIENTED_EDGE('',*,*,#2860,.F.);
#3743=ORIENTED_EDGE('',*,*,#2861,.F.);
#3744=ORIENTED_EDGE('',*,*,#2862,.T.);
#3745=ORIENTED_EDGE('',*,*,#2863,.F.);
#3746=ORIENTED_EDGE('',*,*,#2862,.F.);
#3747=ORIENTED_EDGE('',*,*,#2864,.F.);
#3748=ORIENTED_EDGE('',*,*,#2865,.T.);
#3749=ORIENTED_EDGE('',*,*,#2866,.F.);
#3750=ORIENTED_EDGE('',*,*,#2865,.F.);
#3751=ORIENTED_EDGE('',*,*,#2867,.F.);
#3752=ORIENTED_EDGE('',*,*,#2868,.T.);
#3753=ORIENTED_EDGE('',*,*,#2869,.F.);
#3754=ORIENTED_EDGE('',*,*,#2868,.F.);
#3755=ORIENTED_EDGE('',*,*,#2870,.F.);
#3756=ORIENTED_EDGE('',*,*,#2871,.T.);
#3757=ORIENTED_EDGE('',*,*,#2872,.F.);
#3758=ORIENTED_EDGE('',*,*,#2871,.F.);
#3759=ORIENTED_EDGE('',*,*,#2873,.F.);
#3760=ORIENTED_EDGE('',*,*,#2874,.T.);
#3761=ORIENTED_EDGE('',*,*,#2875,.F.);
#3762=ORIENTED_EDGE('',*,*,#2874,.F.);
#3763=ORIENTED_EDGE('',*,*,#2876,.F.);
#3764=ORIENTED_EDGE('',*,*,#2877,.T.);
#3765=ORIENTED_EDGE('',*,*,#2878,.F.);
#3766=ORIENTED_EDGE('',*,*,#2877,.F.);
#3767=ORIENTED_EDGE('',*,*,#2879,.F.);
#3768=ORIENTED_EDGE('',*,*,#2880,.T.);
#3769=ORIENTED_EDGE('',*,*,#2881,.F.);
#3770=ORIENTED_EDGE('',*,*,#2880,.F.);
#3771=ORIENTED_EDGE('',*,*,#2882,.F.);
#3772=ORIENTED_EDGE('',*,*,#2883,.T.);
#3773=ORIENTED_EDGE('',*,*,#2884,.F.);
#3774=ORIENTED_EDGE('',*,*,#2883,.F.);
#3775=ORIENTED_EDGE('',*,*,#2885,.F.);
#3776=ORIENTED_EDGE('',*,*,#2886,.T.);
#3777=ORIENTED_EDGE('',*,*,#2886,.F.);
#3778=ORIENTED_EDGE('',*,*,#2887,.T.);
#3779=ORIENTED_EDGE('',*,*,#2888,.T.);
#3780=ORIENTED_EDGE('',*,*,#2887,.F.);
#3781=ORIENTED_EDGE('',*,*,#2889,.F.);
#3782=ORIENTED_EDGE('',*,*,#2888,.F.);
#3783=ORIENTED_EDGE('',*,*,#2890,.F.);
#3784=ORIENTED_EDGE('',*,*,#2813,.T.);
#3785=ORIENTED_EDGE('',*,*,#2816,.T.);
#3786=ORIENTED_EDGE('',*,*,#2819,.T.);
#3787=ORIENTED_EDGE('',*,*,#2822,.T.);
#3788=ORIENTED_EDGE('',*,*,#2825,.T.);
#3789=ORIENTED_EDGE('',*,*,#2828,.T.);
#3790=ORIENTED_EDGE('',*,*,#2831,.T.);
#3791=ORIENTED_EDGE('',*,*,#2834,.T.);
#3792=ORIENTED_EDGE('',*,*,#2837,.T.);
#3793=ORIENTED_EDGE('',*,*,#2840,.T.);
#3794=ORIENTED_EDGE('',*,*,#2843,.T.);
#3795=ORIENTED_EDGE('',*,*,#2846,.T.);
#3796=ORIENTED_EDGE('',*,*,#2891,.T.);
#3797=ORIENTED_EDGE('',*,*,#2882,.T.);
#3798=ORIENTED_EDGE('',*,*,#2879,.T.);
#3799=ORIENTED_EDGE('',*,*,#2876,.T.);
#3800=ORIENTED_EDGE('',*,*,#2873,.T.);
#3801=ORIENTED_EDGE('',*,*,#2870,.T.);
#3802=ORIENTED_EDGE('',*,*,#2867,.T.);
#3803=ORIENTED_EDGE('',*,*,#2864,.T.);
#3804=ORIENTED_EDGE('',*,*,#2861,.T.);
#3805=ORIENTED_EDGE('',*,*,#2810,.T.);
#3806=ORIENTED_EDGE('',*,*,#2807,.T.);
#3807=ORIENTED_EDGE('',*,*,#2804,.T.);
#3808=ORIENTED_EDGE('',*,*,#2801,.T.);
#3809=ORIENTED_EDGE('',*,*,#2892,.F.);
#3810=ORIENTED_EDGE('',*,*,#2893,.T.);
#3811=ORIENTED_EDGE('',*,*,#2885,.T.);
#3812=ORIENTED_EDGE('',*,*,#2893,.F.);
#3813=ORIENTED_EDGE('',*,*,#2894,.F.);
#3814=ORIENTED_EDGE('',*,*,#2895,.T.);
#3815=ORIENTED_EDGE('',*,*,#2890,.T.);
#3816=ORIENTED_EDGE('',*,*,#2895,.F.);
#3817=ORIENTED_EDGE('',*,*,#2894,.T.);
#3818=ORIENTED_EDGE('',*,*,#2892,.T.);
#3819=ORIENTED_EDGE('',*,*,#2884,.T.);
#3820=ORIENTED_EDGE('',*,*,#2881,.T.);
#3821=ORIENTED_EDGE('',*,*,#2878,.T.);
#3822=ORIENTED_EDGE('',*,*,#2875,.T.);
#3823=ORIENTED_EDGE('',*,*,#2872,.T.);
#3824=ORIENTED_EDGE('',*,*,#2869,.T.);
#3825=ORIENTED_EDGE('',*,*,#2866,.T.);
#3826=ORIENTED_EDGE('',*,*,#2863,.T.);
#3827=ORIENTED_EDGE('',*,*,#2889,.T.);
#3828=ORIENTED_EDGE('',*,*,#2896,.T.);
#3829=ORIENTED_EDGE('',*,*,#2897,.T.);
#3830=ORIENTED_EDGE('',*,*,#2896,.F.);
#3831=ORIENTED_EDGE('',*,*,#2891,.F.);
#3832=ORIENTED_EDGE('',*,*,#2898,.T.);
#3833=ORIENTED_EDGE('',*,*,#2899,.T.);
#3834=ORIENTED_EDGE('',*,*,#2898,.F.);
#3835=ORIENTED_EDGE('',*,*,#2899,.F.);
#3836=ORIENTED_EDGE('',*,*,#2897,.F.);
#3837=ORIENTED_EDGE('',*,*,#2858,.T.);
#3838=ORIENTED_EDGE('',*,*,#2855,.T.);
#3839=ORIENTED_EDGE('',*,*,#2852,.T.);
#3840=ORIENTED_EDGE('',*,*,#2849,.T.);
#3841=ORIENTED_EDGE('',*,*,#2900,.F.);
#3842=ORIENTED_EDGE('',*,*,#2901,.T.);
#3843=ORIENTED_EDGE('',*,*,#2902,.T.);
#3844=ORIENTED_EDGE('',*,*,#2901,.F.);
#3845=ORIENTED_EDGE('',*,*,#2903,.F.);
#3846=ORIENTED_EDGE('',*,*,#2904,.T.);
#3847=ORIENTED_EDGE('',*,*,#2905,.T.);
#3848=ORIENTED_EDGE('',*,*,#2904,.F.);
#3849=ORIENTED_EDGE('',*,*,#2903,.T.);
#3850=ORIENTED_EDGE('',*,*,#2900,.T.);
#3851=ORIENTED_EDGE('',*,*,#2905,.F.);
#3852=ORIENTED_EDGE('',*,*,#2902,.F.);
#3853=ORIENTED_EDGE('',*,*,#2906,.F.);
#3854=ORIENTED_EDGE('',*,*,#2907,.T.);
#3855=ORIENTED_EDGE('',*,*,#2908,.F.);
#3856=ORIENTED_EDGE('',*,*,#2907,.F.);
#3857=ORIENTED_EDGE('',*,*,#2909,.F.);
#3858=ORIENTED_EDGE('',*,*,#2910,.T.);
#3859=ORIENTED_EDGE('',*,*,#2911,.F.);
#3860=ORIENTED_EDGE('',*,*,#2910,.F.);
#3861=ORIENTED_EDGE('',*,*,#2912,.F.);
#3862=ORIENTED_EDGE('',*,*,#2913,.T.);
#3863=ORIENTED_EDGE('',*,*,#2914,.F.);
#3864=ORIENTED_EDGE('',*,*,#2913,.F.);
#3865=ORIENTED_EDGE('',*,*,#2915,.F.);
#3866=ORIENTED_EDGE('',*,*,#2916,.T.);
#3867=ORIENTED_EDGE('',*,*,#2917,.F.);
#3868=ORIENTED_EDGE('',*,*,#2916,.F.);
#3869=ORIENTED_EDGE('',*,*,#2918,.F.);
#3870=ORIENTED_EDGE('',*,*,#2919,.T.);
#3871=ORIENTED_EDGE('',*,*,#2920,.F.);
#3872=ORIENTED_EDGE('',*,*,#2919,.F.);
#3873=ORIENTED_EDGE('',*,*,#2918,.T.);
#3874=ORIENTED_EDGE('',*,*,#2921,.T.);
#3875=ORIENTED_EDGE('',*,*,#2921,.F.);
#3876=ORIENTED_EDGE('',*,*,#2922,.T.);
#3877=ORIENTED_EDGE('',*,*,#2923,.T.);
#3878=ORIENTED_EDGE('',*,*,#2922,.F.);
#3879=ORIENTED_EDGE('',*,*,#2924,.F.);
#3880=ORIENTED_EDGE('',*,*,#2925,.T.);
#3881=ORIENTED_EDGE('',*,*,#2926,.T.);
#3882=ORIENTED_EDGE('',*,*,#2925,.F.);
#3883=ORIENTED_EDGE('',*,*,#2924,.T.);
#3884=ORIENTED_EDGE('',*,*,#2920,.T.);
#3885=ORIENTED_EDGE('',*,*,#2917,.T.);
#3886=ORIENTED_EDGE('',*,*,#2914,.T.);
#3887=ORIENTED_EDGE('',*,*,#2911,.T.);
#3888=ORIENTED_EDGE('',*,*,#2908,.T.);
#3889=ORIENTED_EDGE('',*,*,#2926,.F.);
#3890=ORIENTED_EDGE('',*,*,#2923,.F.);
#3891=ORIENTED_EDGE('',*,*,#2915,.T.);
#3892=ORIENTED_EDGE('',*,*,#2912,.T.);
#3893=ORIENTED_EDGE('',*,*,#2909,.T.);
#3894=ORIENTED_EDGE('',*,*,#2906,.T.);
#3895=ORIENTED_EDGE('',*,*,#2927,.F.);
#3896=ORIENTED_EDGE('',*,*,#2928,.T.);
#3897=ORIENTED_EDGE('',*,*,#2929,.F.);
#3898=ORIENTED_EDGE('',*,*,#2928,.F.);
#3899=ORIENTED_EDGE('',*,*,#2930,.F.);
#3900=ORIENTED_EDGE('',*,*,#2931,.T.);
#3901=ORIENTED_EDGE('',*,*,#2932,.F.);
#3902=ORIENTED_EDGE('',*,*,#2931,.F.);
#3903=ORIENTED_EDGE('',*,*,#2933,.F.);
#3904=ORIENTED_EDGE('',*,*,#2934,.T.);
#3905=ORIENTED_EDGE('',*,*,#2935,.F.);
#3906=ORIENTED_EDGE('',*,*,#2934,.F.);
#3907=ORIENTED_EDGE('',*,*,#2936,.F.);
#3908=ORIENTED_EDGE('',*,*,#2937,.T.);
#3909=ORIENTED_EDGE('',*,*,#2938,.F.);
#3910=ORIENTED_EDGE('',*,*,#2937,.F.);
#3911=ORIENTED_EDGE('',*,*,#2939,.F.);
#3912=ORIENTED_EDGE('',*,*,#2940,.T.);
#3913=ORIENTED_EDGE('',*,*,#2941,.F.);
#3914=ORIENTED_EDGE('',*,*,#2940,.F.);
#3915=ORIENTED_EDGE('',*,*,#2942,.F.);
#3916=ORIENTED_EDGE('',*,*,#2943,.T.);
#3917=ORIENTED_EDGE('',*,*,#2944,.F.);
#3918=ORIENTED_EDGE('',*,*,#2943,.F.);
#3919=ORIENTED_EDGE('',*,*,#2945,.F.);
#3920=ORIENTED_EDGE('',*,*,#2946,.T.);
#3921=ORIENTED_EDGE('',*,*,#2947,.F.);
#3922=ORIENTED_EDGE('',*,*,#2946,.F.);
#3923=ORIENTED_EDGE('',*,*,#2948,.F.);
#3924=ORIENTED_EDGE('',*,*,#2949,.T.);
#3925=ORIENTED_EDGE('',*,*,#2950,.F.);
#3926=ORIENTED_EDGE('',*,*,#2949,.F.);
#3927=ORIENTED_EDGE('',*,*,#2951,.F.);
#3928=ORIENTED_EDGE('',*,*,#2952,.T.);
#3929=ORIENTED_EDGE('',*,*,#2953,.F.);
#3930=ORIENTED_EDGE('',*,*,#2952,.F.);
#3931=ORIENTED_EDGE('',*,*,#2954,.F.);
#3932=ORIENTED_EDGE('',*,*,#2955,.T.);
#3933=ORIENTED_EDGE('',*,*,#2956,.F.);
#3934=ORIENTED_EDGE('',*,*,#2955,.F.);
#3935=ORIENTED_EDGE('',*,*,#2957,.F.);
#3936=ORIENTED_EDGE('',*,*,#2958,.T.);
#3937=ORIENTED_EDGE('',*,*,#2959,.F.);
#3938=ORIENTED_EDGE('',*,*,#2958,.F.);
#3939=ORIENTED_EDGE('',*,*,#2960,.F.);
#3940=ORIENTED_EDGE('',*,*,#2961,.T.);
#3941=ORIENTED_EDGE('',*,*,#2962,.F.);
#3942=ORIENTED_EDGE('',*,*,#2961,.F.);
#3943=ORIENTED_EDGE('',*,*,#2963,.F.);
#3944=ORIENTED_EDGE('',*,*,#2964,.T.);
#3945=ORIENTED_EDGE('',*,*,#2965,.F.);
#3946=ORIENTED_EDGE('',*,*,#2964,.F.);
#3947=ORIENTED_EDGE('',*,*,#2966,.F.);
#3948=ORIENTED_EDGE('',*,*,#2967,.T.);
#3949=ORIENTED_EDGE('',*,*,#2968,.F.);
#3950=ORIENTED_EDGE('',*,*,#2967,.F.);
#3951=ORIENTED_EDGE('',*,*,#2969,.F.);
#3952=ORIENTED_EDGE('',*,*,#2970,.T.);
#3953=ORIENTED_EDGE('',*,*,#2971,.F.);
#3954=ORIENTED_EDGE('',*,*,#2970,.F.);
#3955=ORIENTED_EDGE('',*,*,#2972,.F.);
#3956=ORIENTED_EDGE('',*,*,#2973,.T.);
#3957=ORIENTED_EDGE('',*,*,#2974,.F.);
#3958=ORIENTED_EDGE('',*,*,#2973,.F.);
#3959=ORIENTED_EDGE('',*,*,#2975,.F.);
#3960=ORIENTED_EDGE('',*,*,#2976,.T.);
#3961=ORIENTED_EDGE('',*,*,#2977,.T.);
#3962=ORIENTED_EDGE('',*,*,#2976,.F.);
#3963=ORIENTED_EDGE('',*,*,#2978,.F.);
#3964=ORIENTED_EDGE('',*,*,#2979,.T.);
#3965=ORIENTED_EDGE('',*,*,#2980,.T.);
#3966=ORIENTED_EDGE('',*,*,#2979,.F.);
#3967=ORIENTED_EDGE('',*,*,#2978,.T.);
#3968=ORIENTED_EDGE('',*,*,#2941,.T.);
#3969=ORIENTED_EDGE('',*,*,#2944,.T.);
#3970=ORIENTED_EDGE('',*,*,#2947,.T.);
#3971=ORIENTED_EDGE('',*,*,#2950,.T.);
#3972=ORIENTED_EDGE('',*,*,#2953,.T.);
#3973=ORIENTED_EDGE('',*,*,#2956,.T.);
#3974=ORIENTED_EDGE('',*,*,#2959,.T.);
#3975=ORIENTED_EDGE('',*,*,#2962,.T.);
#3976=ORIENTED_EDGE('',*,*,#2965,.T.);
#3977=ORIENTED_EDGE('',*,*,#2968,.T.);
#3978=ORIENTED_EDGE('',*,*,#2971,.T.);
#3979=ORIENTED_EDGE('',*,*,#2974,.T.);
#3980=ORIENTED_EDGE('',*,*,#2975,.T.);
#3981=ORIENTED_EDGE('',*,*,#2938,.T.);
#3982=ORIENTED_EDGE('',*,*,#2935,.T.);
#3983=ORIENTED_EDGE('',*,*,#2932,.T.);
#3984=ORIENTED_EDGE('',*,*,#2929,.T.);
#3985=ORIENTED_EDGE('',*,*,#2980,.F.);
#3986=ORIENTED_EDGE('',*,*,#2939,.T.);
#3987=ORIENTED_EDGE('',*,*,#2942,.T.);
#3988=ORIENTED_EDGE('',*,*,#2945,.T.);
#3989=ORIENTED_EDGE('',*,*,#2948,.T.);
#3990=ORIENTED_EDGE('',*,*,#2951,.T.);
#3991=ORIENTED_EDGE('',*,*,#2954,.T.);
#3992=ORIENTED_EDGE('',*,*,#2957,.T.);
#3993=ORIENTED_EDGE('',*,*,#2960,.T.);
#3994=ORIENTED_EDGE('',*,*,#2963,.T.);
#3995=ORIENTED_EDGE('',*,*,#2966,.T.);
#3996=ORIENTED_EDGE('',*,*,#2969,.T.);
#3997=ORIENTED_EDGE('',*,*,#2972,.T.);
#3998=ORIENTED_EDGE('',*,*,#2977,.F.);
#3999=ORIENTED_EDGE('',*,*,#2936,.T.);
#4000=ORIENTED_EDGE('',*,*,#2933,.T.);
#4001=ORIENTED_EDGE('',*,*,#2930,.T.);
#4002=ORIENTED_EDGE('',*,*,#2927,.T.);
#4003=ORIENTED_EDGE('',*,*,#2981,.F.);
#4004=ORIENTED_EDGE('',*,*,#2982,.F.);
#4005=ORIENTED_EDGE('',*,*,#2983,.T.);
#4006=ORIENTED_EDGE('',*,*,#2981,.T.);
#4007=ORIENTED_EDGE('',*,*,#2983,.F.);
#4008=ORIENTED_EDGE('',*,*,#2984,.F.);
#4009=ORIENTED_EDGE('',*,*,#2985,.T.);
#4010=ORIENTED_EDGE('',*,*,#2982,.T.);
#4011=ORIENTED_EDGE('',*,*,#2985,.F.);
#4012=ORIENTED_EDGE('',*,*,#2986,.F.);
#4013=ORIENTED_EDGE('',*,*,#2987,.T.);
#4014=ORIENTED_EDGE('',*,*,#2984,.T.);
#4015=ORIENTED_EDGE('',*,*,#2987,.F.);
#4016=ORIENTED_EDGE('',*,*,#2986,.T.);
#4017=ORIENTED_EDGE('',*,*,#2988,.F.);
#4018=ORIENTED_EDGE('',*,*,#2989,.F.);
#4019=ORIENTED_EDGE('',*,*,#2990,.T.);
#4020=ORIENTED_EDGE('',*,*,#2988,.T.);
#4021=ORIENTED_EDGE('',*,*,#2990,.F.);
#4022=ORIENTED_EDGE('',*,*,#2991,.F.);
#4023=ORIENTED_EDGE('',*,*,#2992,.T.);
#4024=ORIENTED_EDGE('',*,*,#2989,.T.);
#4025=ORIENTED_EDGE('',*,*,#2992,.F.);
#4026=ORIENTED_EDGE('',*,*,#2993,.F.);
#4027=ORIENTED_EDGE('',*,*,#2994,.T.);
#4028=ORIENTED_EDGE('',*,*,#2991,.T.);
#4029=ORIENTED_EDGE('',*,*,#2994,.F.);
#4030=ORIENTED_EDGE('',*,*,#2993,.T.);
#4031=ORIENTED_EDGE('',*,*,#2995,.T.);
#4032=ORIENTED_EDGE('',*,*,#2996,.T.);
#4033=ORIENTED_EDGE('',*,*,#2997,.T.);
#4034=ORIENTED_EDGE('',*,*,#2998,.F.);
#4035=ORIENTED_EDGE('',*,*,#2999,.T.);
#4036=ORIENTED_EDGE('',*,*,#3000,.T.);
#4037=ORIENTED_EDGE('',*,*,#3001,.T.);
#4038=ORIENTED_EDGE('',*,*,#2996,.F.);
#4039=ORIENTED_EDGE('',*,*,#3002,.T.);
#4040=ORIENTED_EDGE('',*,*,#3003,.T.);
#4041=ORIENTED_EDGE('',*,*,#3004,.T.);
#4042=ORIENTED_EDGE('',*,*,#3000,.F.);
#4043=ORIENTED_EDGE('',*,*,#3005,.T.);
#4044=ORIENTED_EDGE('',*,*,#3006,.T.);
#4045=ORIENTED_EDGE('',*,*,#3007,.T.);
#4046=ORIENTED_EDGE('',*,*,#3003,.F.);
#4047=ORIENTED_EDGE('',*,*,#3008,.T.);
#4048=ORIENTED_EDGE('',*,*,#3009,.T.);
#4049=ORIENTED_EDGE('',*,*,#3010,.T.);
#4050=ORIENTED_EDGE('',*,*,#3006,.F.);
#4051=ORIENTED_EDGE('',*,*,#3011,.T.);
#4052=ORIENTED_EDGE('',*,*,#2998,.T.);
#4053=ORIENTED_EDGE('',*,*,#3012,.T.);
#4054=ORIENTED_EDGE('',*,*,#3009,.F.);
#4055=ORIENTED_EDGE('',*,*,#3011,.F.);
#4056=ORIENTED_EDGE('',*,*,#3008,.F.);
#4057=ORIENTED_EDGE('',*,*,#3005,.F.);
#4058=ORIENTED_EDGE('',*,*,#3002,.F.);
#4059=ORIENTED_EDGE('',*,*,#2999,.F.);
#4060=ORIENTED_EDGE('',*,*,#2995,.F.);
#4061=ORIENTED_EDGE('',*,*,#3012,.F.);
#4062=ORIENTED_EDGE('',*,*,#2997,.F.);
#4063=ORIENTED_EDGE('',*,*,#3001,.F.);
#4064=ORIENTED_EDGE('',*,*,#3004,.F.);
#4065=ORIENTED_EDGE('',*,*,#3007,.F.);
#4066=ORIENTED_EDGE('',*,*,#3010,.F.);
#4067=ORIENTED_EDGE('',*,*,#3013,.F.);
#4068=ORIENTED_EDGE('',*,*,#3014,.T.);
#4069=ORIENTED_EDGE('',*,*,#3015,.F.);
#4070=ORIENTED_EDGE('',*,*,#3016,.F.);
#4071=ORIENTED_EDGE('',*,*,#3017,.F.);
#4072=ORIENTED_EDGE('',*,*,#3014,.F.);
#4073=ORIENTED_EDGE('',*,*,#3018,.T.);
#4074=ORIENTED_EDGE('',*,*,#3016,.T.);
#4075=ORIENTED_EDGE('',*,*,#3018,.F.);
#4076=ORIENTED_EDGE('',*,*,#3017,.T.);
#4077=ORIENTED_EDGE('',*,*,#3019,.T.);
#4078=ORIENTED_EDGE('',*,*,#3013,.T.);
#4079=ORIENTED_EDGE('',*,*,#3019,.F.);
#4080=ORIENTED_EDGE('',*,*,#3020,.F.);
#4081=ORIENTED_EDGE('',*,*,#3021,.T.);
#4082=ORIENTED_EDGE('',*,*,#3015,.T.);
#4083=ORIENTED_EDGE('',*,*,#3021,.F.);
#4084=ORIENTED_EDGE('',*,*,#3020,.T.);
#4085=ORIENTED_EDGE('',*,*,#3022,.F.);
#4086=ORIENTED_EDGE('',*,*,#3023,.T.);
#4087=ORIENTED_EDGE('',*,*,#3024,.F.);
#4088=ORIENTED_EDGE('',*,*,#3025,.F.);
#4089=ORIENTED_EDGE('',*,*,#3026,.F.);
#4090=ORIENTED_EDGE('',*,*,#3027,.T.);
#4091=ORIENTED_EDGE('',*,*,#3028,.F.);
#4092=ORIENTED_EDGE('',*,*,#3029,.F.);
#4093=ORIENTED_EDGE('',*,*,#3027,.F.);
#4094=ORIENTED_EDGE('',*,*,#3030,.F.);
#4095=ORIENTED_EDGE('',*,*,#3023,.F.);
#4096=ORIENTED_EDGE('',*,*,#3031,.F.);
#4097=ORIENTED_EDGE('',*,*,#3025,.T.);
#4098=ORIENTED_EDGE('',*,*,#3032,.F.);
#4099=ORIENTED_EDGE('',*,*,#3033,.T.);
#4100=ORIENTED_EDGE('',*,*,#3034,.T.);
#4101=ORIENTED_EDGE('',*,*,#3033,.F.);
#4102=ORIENTED_EDGE('',*,*,#3030,.T.);
#4103=ORIENTED_EDGE('',*,*,#3026,.T.);
#4104=ORIENTED_EDGE('',*,*,#3031,.T.);
#4105=ORIENTED_EDGE('',*,*,#3024,.T.);
#4106=ORIENTED_EDGE('',*,*,#3022,.T.);
#4107=ORIENTED_EDGE('',*,*,#3035,.F.);
#4108=ORIENTED_EDGE('',*,*,#3036,.T.);
#4109=ORIENTED_EDGE('',*,*,#3037,.T.);
#4110=ORIENTED_EDGE('',*,*,#3036,.F.);
#4111=ORIENTED_EDGE('',*,*,#3028,.T.);
#4112=ORIENTED_EDGE('',*,*,#3029,.T.);
#4113=ORIENTED_EDGE('',*,*,#3035,.T.);
#4114=ORIENTED_EDGE('',*,*,#3032,.T.);
#4115=ORIENTED_EDGE('',*,*,#3037,.F.);
#4116=ORIENTED_EDGE('',*,*,#3034,.F.);
#4117=ORIENTED_EDGE('',*,*,#3038,.F.);
#4118=ORIENTED_EDGE('',*,*,#3039,.T.);
#4119=ORIENTED_EDGE('',*,*,#3040,.T.);
#4120=ORIENTED_EDGE('',*,*,#3041,.F.);
#4121=ORIENTED_EDGE('',*,*,#3042,.F.);
#4122=ORIENTED_EDGE('',*,*,#3043,.T.);
#4123=ORIENTED_EDGE('',*,*,#3044,.T.);
#4124=ORIENTED_EDGE('',*,*,#3039,.F.);
#4125=ORIENTED_EDGE('',*,*,#3045,.F.);
#4126=ORIENTED_EDGE('',*,*,#3046,.T.);
#4127=ORIENTED_EDGE('',*,*,#3047,.T.);
#4128=ORIENTED_EDGE('',*,*,#3043,.F.);
#4129=ORIENTED_EDGE('',*,*,#3048,.F.);
#4130=ORIENTED_EDGE('',*,*,#3049,.T.);
#4131=ORIENTED_EDGE('',*,*,#3050,.T.);
#4132=ORIENTED_EDGE('',*,*,#3046,.F.);
#4133=ORIENTED_EDGE('',*,*,#3051,.F.);
#4134=ORIENTED_EDGE('',*,*,#3052,.T.);
#4135=ORIENTED_EDGE('',*,*,#3053,.T.);
#4136=ORIENTED_EDGE('',*,*,#3049,.F.);
#4137=ORIENTED_EDGE('',*,*,#3054,.F.);
#4138=ORIENTED_EDGE('',*,*,#3041,.T.);
#4139=ORIENTED_EDGE('',*,*,#3055,.T.);
#4140=ORIENTED_EDGE('',*,*,#3052,.F.);
#4141=ORIENTED_EDGE('',*,*,#3055,.F.);
#4142=ORIENTED_EDGE('',*,*,#3040,.F.);
#4143=ORIENTED_EDGE('',*,*,#3044,.F.);
#4144=ORIENTED_EDGE('',*,*,#3047,.F.);
#4145=ORIENTED_EDGE('',*,*,#3050,.F.);
#4146=ORIENTED_EDGE('',*,*,#3053,.F.);
#4147=ORIENTED_EDGE('',*,*,#3056,.F.);
#4148=ORIENTED_EDGE('',*,*,#3038,.T.);
#4149=ORIENTED_EDGE('',*,*,#3054,.T.);
#4150=ORIENTED_EDGE('',*,*,#3051,.T.);
#4151=ORIENTED_EDGE('',*,*,#3048,.T.);
#4152=ORIENTED_EDGE('',*,*,#3045,.T.);
#4153=ORIENTED_EDGE('',*,*,#3042,.T.);
#4154=ORIENTED_EDGE('',*,*,#3057,.F.);
#4155=ORIENTED_EDGE('',*,*,#3058,.T.);
#4156=ORIENTED_EDGE('',*,*,#3056,.T.);
#4157=ORIENTED_EDGE('',*,*,#3058,.F.);
#4158=ORIENTED_EDGE('',*,*,#3059,.F.);
#4159=ORIENTED_EDGE('',*,*,#3060,.T.);
#4160=ORIENTED_EDGE('',*,*,#3057,.T.);
#4161=ORIENTED_EDGE('',*,*,#3060,.F.);
#4162=ORIENTED_EDGE('',*,*,#3061,.F.);
#4163=ORIENTED_EDGE('',*,*,#3062,.T.);
#4164=ORIENTED_EDGE('',*,*,#3059,.T.);
#4165=ORIENTED_EDGE('',*,*,#3062,.F.);
#4166=ORIENTED_EDGE('',*,*,#3061,.T.);
#4167=CYLINDRICAL_SURFACE('',#4910,0.165);
#4168=CYLINDRICAL_SURFACE('',#4913,0.165);
#4169=CYLINDRICAL_SURFACE('',#4916,0.31);
#4170=CYLINDRICAL_SURFACE('',#4919,0.25);
#4171=CYLINDRICAL_SURFACE('',#4922,0.25);
#4172=CYLINDRICAL_SURFACE('',#4925,0.25);
#4173=CYLINDRICAL_SURFACE('',#4928,0.25);
#4174=CYLINDRICAL_SURFACE('',#4938,1.);
#4175=CYLINDRICAL_SURFACE('',#4944,1.);
#4176=CYLINDRICAL_SURFACE('',#4950,1.);
#4177=CYLINDRICAL_SURFACE('',#4956,1.);
#4178=CYLINDRICAL_SURFACE('',#4962,0.33);
#4179=CYLINDRICAL_SURFACE('',#4965,0.33);
#4180=CYLINDRICAL_SURFACE('',#4968,0.33);
#4181=CYLINDRICAL_SURFACE('',#4971,0.33);
#4182=CYLINDRICAL_SURFACE('',#4980,1.6);
#4183=CYLINDRICAL_SURFACE('',#4981,1.25);
#4184=CYLINDRICAL_SURFACE('',#4985,3.5);
#4185=CYLINDRICAL_SURFACE('',#4987,1.25);
#4186=CYLINDRICAL_SURFACE('',#4992,1.255);
#4187=CYLINDRICAL_SURFACE('',#4995,1.7);
#4188=CYLINDRICAL_SURFACE('',#5003,0.21);
#4189=CYLINDRICAL_SURFACE('',#5006,1.255);
#4190=CYLINDRICAL_SURFACE('',#5009,1.8);
#4191=CYLINDRICAL_SURFACE('',#5015,0.225);
#4192=CYLINDRICAL_SURFACE('',#5018,0.225);
#4193=CYLINDRICAL_SURFACE('',#5021,0.999999999999999);
#4194=CYLINDRICAL_SURFACE('',#5026,0.31);
#4195=CYLINDRICAL_SURFACE('',#5028,2.);
#4196=CYLINDRICAL_SURFACE('',#5034,0.31);
#4197=CYLINDRICAL_SURFACE('',#5039,0.6);
#4198=CYLINDRICAL_SURFACE('',#5041,0.999999999999999);
#4199=CYLINDRICAL_SURFACE('',#5052,0.32);
#4200=CYLINDRICAL_SURFACE('',#5055,0.6);
#4201=CYLINDRICAL_SURFACE('',#5075,0.5);
#4202=CYLINDRICAL_SURFACE('',#5083,0.2942);
#4203=CYLINDRICAL_SURFACE('',#5092,1.88531);
#4204=CYLINDRICAL_SURFACE('',#5094,1.25);
#4205=CYLINDRICAL_SURFACE('',#5100,1.88531);
#4206=CYLINDRICAL_SURFACE('',#5112,1.96469);
#4207=CYLINDRICAL_SURFACE('',#5119,2.6);
#4208=CYLINDRICAL_SURFACE('',#5124,1.96469);
#4209=CYLINDRICAL_SURFACE('',#5148,1.956752);
#4210=CYLINDRICAL_SURFACE('',#5196,1.893248);
#4211=CYLINDRICAL_SURFACE('',#5210,1.95469);
#4212=CYLINDRICAL_SURFACE('',#5214,1.90031);
#4213=CYLINDRICAL_SURFACE('',#5218,1.95469);
#4214=CYLINDRICAL_SURFACE('',#5222,1.90031);
#4215=CYLINDRICAL_SURFACE('',#5242,0.24505);
#4216=CYLINDRICAL_SURFACE('',#5245,0.165);
#4217=CYLINDRICAL_SURFACE('',#5249,0.165);
#4218=CYLINDRICAL_SURFACE('',#5253,0.165);
#4219=CYLINDRICAL_SURFACE('',#5257,0.165);
#4220=CYLINDRICAL_SURFACE('',#5261,0.31);
#4221=CYLINDRICAL_SURFACE('',#5265,0.31);
#4222=CYLINDRICAL_SURFACE('',#5269,0.31);
#4223=CYLINDRICAL_SURFACE('',#5273,0.31);
#4224=CYLINDRICAL_SURFACE('',#5277,0.31);
#4225=CYLINDRICAL_SURFACE('',#5281,0.31);
#4226=CYLINDRICAL_SURFACE('',#5285,0.31);
#4227=CYLINDRICAL_SURFACE('',#5289,0.31);
#4228=CYLINDRICAL_SURFACE('',#5293,0.31);
#4229=CYLINDRICAL_SURFACE('',#5297,0.31);
#4230=CYLINDRICAL_SURFACE('',#5301,0.31);
#4231=CYLINDRICAL_SURFACE('',#5305,0.31);
#4232=CYLINDRICAL_SURFACE('',#5309,0.165);
#4233=CYLINDRICAL_SURFACE('',#5313,0.165);
#4234=CYLINDRICAL_SURFACE('',#5317,0.165);
#4235=CYLINDRICAL_SURFACE('',#5321,0.165);
#4236=CYLINDRICAL_SURFACE('',#5325,0.33);
#4237=CYLINDRICAL_SURFACE('',#5328,0.33);
#4238=CYLINDRICAL_SURFACE('',#5331,0.33);
#4239=CYLINDRICAL_SURFACE('',#5334,0.33);
#4240=CYLINDRICAL_SURFACE('',#5337,0.33);
#4241=CYLINDRICAL_SURFACE('',#5340,0.33);
#4242=CYLINDRICAL_SURFACE('',#5343,0.33);
#4243=CYLINDRICAL_SURFACE('',#5346,0.33);
#4244=CYLINDRICAL_SURFACE('',#5352,1.9);
#4245=CYLINDRICAL_SURFACE('',#5359,2.);
#4246=CYLINDRICAL_SURFACE('',#5361,10.);
#4247=CYLINDRICAL_SURFACE('',#5364,2.6);
#4248=CYLINDRICAL_SURFACE('',#5366,4.);
#4249=CYLINDRICAL_SURFACE('',#5370,2.);
#4250=CYLINDRICAL_SURFACE('',#5373,2.59);
#4251=CYLINDRICAL_SURFACE('',#5379,0.225);
#4252=CYLINDRICAL_SURFACE('',#5382,0.225);
#4253=CYLINDRICAL_SURFACE('',#5385,0.225);
#4254=CYLINDRICAL_SURFACE('',#5388,0.225);
#4255=CYLINDRICAL_SURFACE('',#5391,2.59);
#4256=CYLINDRICAL_SURFACE('',#5396,1.9);
#4257=CYLINDRICAL_SURFACE('',#5398,4.);
#4258=CYLINDRICAL_SURFACE('',#5404,0.225);
#4259=CYLINDRICAL_SURFACE('',#5407,0.225);
#4260=CYLINDRICAL_SURFACE('',#5410,0.225);
#4261=CYLINDRICAL_SURFACE('',#5413,0.225);
#4262=CYLINDRICAL_SURFACE('',#5416,0.31);
#4263=CYLINDRICAL_SURFACE('',#5419,0.31);
#4264=CYLINDRICAL_SURFACE('',#5422,0.31);
#4265=CYLINDRICAL_SURFACE('',#5425,0.31);
#4266=CYLINDRICAL_SURFACE('',#5428,0.31);
#4267=CYLINDRICAL_SURFACE('',#5431,0.31);
#4268=CYLINDRICAL_SURFACE('',#5434,0.31);
#4269=CYLINDRICAL_SURFACE('',#5437,0.31);
#4270=CYLINDRICAL_SURFACE('',#5440,0.31);
#4271=CYLINDRICAL_SURFACE('',#5443,0.31);
#4272=CYLINDRICAL_SURFACE('',#5446,0.31);
#4273=CYLINDRICAL_SURFACE('',#5449,0.31);
#4274=CYLINDRICAL_SURFACE('',#5452,6.5);
#4275=CYLINDRICAL_SURFACE('',#5455,8.);
#4276=CYLINDRICAL_SURFACE('',#5465,0.35);
#4277=CYLINDRICAL_SURFACE('',#5473,0.1954);
#4278=CYLINDRICAL_SURFACE('',#5531,0.5);
#4279=CYLINDRICAL_SURFACE('',#5532,0.3);
#4280=CYLINDRICAL_SURFACE('',#5533,0.3);
#4281=CYLINDRICAL_SURFACE('',#5539,0.21);
#4282=CYLINDRICAL_SURFACE('',#5542,0.3);
#4283=CYLINDRICAL_SURFACE('',#5545,1.2);
#4284=CYLINDRICAL_SURFACE('',#5562,0.24505);
#4285=ADVANCED_FACE('',(#670),#4167,.F.);
#4286=ADVANCED_FACE('',(#671),#4168,.F.);
#4287=ADVANCED_FACE('',(#672),#4169,.F.);
#4288=ADVANCED_FACE('',(#673),#4170,.F.);
#4289=ADVANCED_FACE('',(#674),#4171,.F.);
#4290=ADVANCED_FACE('',(#675),#4172,.F.);
#4291=ADVANCED_FACE('',(#676),#4173,.F.);
#4292=ADVANCED_FACE('',(#677),#537,.T.);
#4293=ADVANCED_FACE('',(#678),#538,.T.);
#4294=ADVANCED_FACE('',(#679),#539,.T.);
#4295=ADVANCED_FACE('',(#680),#540,.T.);
#4296=ADVANCED_FACE('',(#681,#387,#388,#389,#390,#391,#392,#393),#541,.T.);
#4297=ADVANCED_FACE('',(#682,#394,#395,#396,#397,#398,#399,#400),#542,.F.);
#4298=ADVANCED_FACE('',(#683),#4174,.T.);
#4299=ADVANCED_FACE('',(#684),#543,.T.);
#4300=ADVANCED_FACE('',(#685),#544,.F.);
#4301=ADVANCED_FACE('',(#686),#4175,.T.);
#4302=ADVANCED_FACE('',(#687),#545,.T.);
#4303=ADVANCED_FACE('',(#688),#546,.F.);
#4304=ADVANCED_FACE('',(#689),#4176,.T.);
#4305=ADVANCED_FACE('',(#690),#547,.T.);
#4306=ADVANCED_FACE('',(#691),#548,.F.);
#4307=ADVANCED_FACE('',(#692),#4177,.T.);
#4308=ADVANCED_FACE('',(#693),#549,.T.);
#4309=ADVANCED_FACE('',(#694),#550,.F.);
#4310=ADVANCED_FACE('',(#695),#4178,.F.);
#4311=ADVANCED_FACE('',(#696),#4179,.F.);
#4312=ADVANCED_FACE('',(#697),#4180,.F.);
#4313=ADVANCED_FACE('',(#698),#4181,.F.);
#4314=ADVANCED_FACE('',(#699,#401),#551,.T.);
#4315=ADVANCED_FACE('',(#700,#402),#552,.F.);
#4316=ADVANCED_FACE('',(#701),#4182,.T.);
#4317=ADVANCED_FACE('',(#702),#4183,.T.);
#4318=ADVANCED_FACE('',(#703,#403,#404,#405,#406,#407),#553,.T.);
#4319=ADVANCED_FACE('',(#704),#4184,.T.);
#4320=ADVANCED_FACE('',(#705),#4185,.T.);
#4321=ADVANCED_FACE('',(#706),#554,.T.);
#4322=ADVANCED_FACE('',(#707,#408,#409,#410,#411),#555,.F.);
#4323=ADVANCED_FACE('',(#708),#4186,.F.);
#4324=ADVANCED_FACE('',(#709),#4187,.T.);
#4325=ADVANCED_FACE('',(#710,#412),#556,.T.);
#4326=ADVANCED_FACE('',(#711,#413),#557,.F.);
#4327=ADVANCED_FACE('',(#712),#558,.T.);
#4328=ADVANCED_FACE('',(#713),#4188,.F.);
#4329=ADVANCED_FACE('',(#714),#559,.T.);
#4330=ADVANCED_FACE('',(#715,#414),#4189,.F.);
#4331=ADVANCED_FACE('',(#716,#415),#4190,.T.);
#4332=ADVANCED_FACE('',(#717,#416),#560,.T.);
#4333=ADVANCED_FACE('',(#718,#417),#561,.F.);
#4334=ADVANCED_FACE('',(#719),#4191,.F.);
#4335=ADVANCED_FACE('',(#720),#4192,.F.);
#4336=ADVANCED_FACE('',(#721),#4193,.F.);
#4337=ADVANCED_FACE('',(#722,#418),#562,.T.);
#4338=ADVANCED_FACE('',(#723),#4194,.F.);
#4339=ADVANCED_FACE('',(#724),#4195,.T.);
#4340=ADVANCED_FACE('',(#725,#419,#420,#421),#563,.T.);
#4341=ADVANCED_FACE('',(#726,#422,#423,#424),#564,.F.);
#4342=ADVANCED_FACE('',(#727),#4196,.F.);
#4343=ADVANCED_FACE('',(#728,#425),#565,.F.);
#4344=ADVANCED_FACE('',(#729),#4197,.F.);
#4345=ADVANCED_FACE('',(#730),#4198,.T.);
#4346=ADVANCED_FACE('',(#731,#426),#566,.T.);
#4347=ADVANCED_FACE('',(#732,#427),#567,.F.);
#4348=ADVANCED_FACE('',(#733),#233,.T.);
#4349=ADVANCED_FACE('',(#734),#568,.T.);
#4350=ADVANCED_FACE('',(#735),#569,.F.);
#4351=ADVANCED_FACE('',(#736),#4199,.F.);
#4352=ADVANCED_FACE('',(#737),#4200,.T.);
#4353=ADVANCED_FACE('',(#738,#428),#570,.T.);
#4354=ADVANCED_FACE('',(#739,#429),#571,.F.);
#4355=ADVANCED_FACE('',(#740),#572,.F.);
#4356=ADVANCED_FACE('',(#741),#573,.F.);
#4357=ADVANCED_FACE('',(#742),#574,.F.);
#4358=ADVANCED_FACE('',(#743),#575,.F.);
#4359=ADVANCED_FACE('',(#744),#576,.F.);
#4360=ADVANCED_FACE('',(#745),#577,.F.);
#4361=ADVANCED_FACE('',(#746),#578,.F.);
#4362=ADVANCED_FACE('',(#747),#579,.F.);
#4363=ADVANCED_FACE('',(#748),#580,.F.);
#4364=ADVANCED_FACE('',(#749),#581,.T.);
#4365=ADVANCED_FACE('',(#750),#215,.T.);
#4366=ADVANCED_FACE('',(#751),#4201,.T.);
#4367=ADVANCED_FACE('',(#752),#216,.T.);
#4368=ADVANCED_FACE('',(#753,#430),#582,.T.);
#4369=ADVANCED_FACE('',(#754),#217,.T.);
#4370=ADVANCED_FACE('',(#755),#4202,.T.);
#4371=ADVANCED_FACE('',(#756),#213,.F.);
#4372=ADVANCED_FACE('',(#757),#4203,.T.);
#4373=ADVANCED_FACE('',(#758),#4204,.F.);
#4374=ADVANCED_FACE('',(#759),#218,.F.);
#4375=ADVANCED_FACE('',(#760,#431),#583,.T.);
#4376=ADVANCED_FACE('',(#761),#4205,.T.);
#4377=ADVANCED_FACE('',(#762,#432),#584,.T.);
#4378=ADVANCED_FACE('',(#763),#219,.F.);
#4379=ADVANCED_FACE('',(#764),#214,.F.);
#4380=ADVANCED_FACE('',(#765),#4206,.F.);
#4381=ADVANCED_FACE('',(#766,#433),#585,.T.);
#4382=ADVANCED_FACE('',(#767),#220,.T.);
#4383=ADVANCED_FACE('',(#768),#4207,.T.);
#4384=ADVANCED_FACE('',(#769),#221,.T.);
#4385=ADVANCED_FACE('',(#770,#434),#586,.T.);
#4386=ADVANCED_FACE('',(#771),#4208,.F.);
#4387=ADVANCED_FACE('',(#772),#195,.T.);
#4388=ADVANCED_FACE('',(#773),#196,.T.);
#4389=ADVANCED_FACE('',(#774),#197,.T.);
#4390=ADVANCED_FACE('',(#775),#198,.T.);
#4391=ADVANCED_FACE('',(#776),#199,.T.);
#4392=ADVANCED_FACE('',(#777),#200,.T.);
#4393=ADVANCED_FACE('',(#778),#201,.T.);
#4394=ADVANCED_FACE('',(#779),#202,.T.);
#4395=ADVANCED_FACE('',(#780),#203,.T.);
#4396=ADVANCED_FACE('',(#781),#204,.F.);
#4397=ADVANCED_FACE('',(#782),#4209,.T.);
#4398=ADVANCED_FACE('',(#783),#587,.T.);
#4399=ADVANCED_FACE('',(#784),#205,.F.);
#4400=ADVANCED_FACE('',(#785),#588,.T.);
#4401=ADVANCED_FACE('',(#786),#206,.F.);
#4402=ADVANCED_FACE('',(#787),#589,.T.);
#4403=ADVANCED_FACE('',(#788),#207,.F.);
#4404=ADVANCED_FACE('',(#789),#590,.T.);
#4405=ADVANCED_FACE('',(#790),#208,.F.);
#4406=ADVANCED_FACE('',(#791),#591,.T.);
#4407=ADVANCED_FACE('',(#792),#209,.F.);
#4408=ADVANCED_FACE('',(#793),#592,.T.);
#4409=ADVANCED_FACE('',(#794),#210,.F.);
#4410=ADVANCED_FACE('',(#795),#593,.T.);
#4411=ADVANCED_FACE('',(#796),#211,.F.);
#4412=ADVANCED_FACE('',(#797),#4210,.F.);
#4413=ADVANCED_FACE('',(#798),#594,.T.);
#4414=ADVANCED_FACE('',(#799),#212,.F.);
#4415=ADVANCED_FACE('',(#800,#435),#595,.T.);
#4416=ADVANCED_FACE('',(#801),#596,.T.);
#4417=ADVANCED_FACE('',(#802,#436),#597,.T.);
#4418=ADVANCED_FACE('',(#803),#4211,.T.);
#4419=ADVANCED_FACE('',(#804,#437),#598,.T.);
#4420=ADVANCED_FACE('',(#805),#4212,.F.);
#4421=ADVANCED_FACE('',(#806,#438),#599,.T.);
#4422=ADVANCED_FACE('',(#807),#4213,.T.);
#4423=ADVANCED_FACE('',(#808,#439),#600,.T.);
#4424=ADVANCED_FACE('',(#809),#4214,.F.);
#4425=ADVANCED_FACE('',(#810),#601,.F.);
#4426=ADVANCED_FACE('',(#811),#602,.F.);
#4427=ADVANCED_FACE('',(#812),#603,.F.);
#4428=ADVANCED_FACE('',(#813),#604,.F.);
#4429=ADVANCED_FACE('',(#814),#605,.F.);
#4430=ADVANCED_FACE('',(#815),#606,.F.);
#4431=ADVANCED_FACE('',(#816),#607,.F.);
#4432=ADVANCED_FACE('',(#817),#608,.F.);
#4433=ADVANCED_FACE('',(#818,#440),#609,.T.);
#4434=ADVANCED_FACE('',(#819),#222,.T.);
#4435=ADVANCED_FACE('',(#820),#4215,.T.);
#4436=ADVANCED_FACE('',(#821),#4216,.F.);
#4437=ADVANCED_FACE('',(#822),#610,.F.);
#4438=ADVANCED_FACE('',(#823),#4217,.F.);
#4439=ADVANCED_FACE('',(#824),#611,.F.);
#4440=ADVANCED_FACE('',(#825),#4218,.F.);
#4441=ADVANCED_FACE('',(#826),#612,.F.);
#4442=ADVANCED_FACE('',(#827),#4219,.F.);
#4443=ADVANCED_FACE('',(#828),#613,.F.);
#4444=ADVANCED_FACE('',(#829),#4220,.F.);
#4445=ADVANCED_FACE('',(#830),#614,.F.);
#4446=ADVANCED_FACE('',(#831),#4221,.F.);
#4447=ADVANCED_FACE('',(#832),#615,.F.);
#4448=ADVANCED_FACE('',(#833),#4222,.F.);
#4449=ADVANCED_FACE('',(#834),#616,.F.);
#4450=ADVANCED_FACE('',(#835),#4223,.F.);
#4451=ADVANCED_FACE('',(#836),#617,.F.);
#4452=ADVANCED_FACE('',(#837),#4224,.F.);
#4453=ADVANCED_FACE('',(#838),#618,.F.);
#4454=ADVANCED_FACE('',(#839),#4225,.F.);
#4455=ADVANCED_FACE('',(#840),#619,.F.);
#4456=ADVANCED_FACE('',(#841),#4226,.F.);
#4457=ADVANCED_FACE('',(#842),#620,.F.);
#4458=ADVANCED_FACE('',(#843),#4227,.F.);
#4459=ADVANCED_FACE('',(#844),#621,.F.);
#4460=ADVANCED_FACE('',(#845),#4228,.F.);
#4461=ADVANCED_FACE('',(#846),#622,.F.);
#4462=ADVANCED_FACE('',(#847),#4229,.F.);
#4463=ADVANCED_FACE('',(#848),#623,.F.);
#4464=ADVANCED_FACE('',(#849),#4230,.F.);
#4465=ADVANCED_FACE('',(#850),#624,.F.);
#4466=ADVANCED_FACE('',(#851),#4231,.F.);
#4467=ADVANCED_FACE('',(#852),#625,.F.);
#4468=ADVANCED_FACE('',(#853),#4232,.F.);
#4469=ADVANCED_FACE('',(#854),#626,.F.);
#4470=ADVANCED_FACE('',(#855),#4233,.F.);
#4471=ADVANCED_FACE('',(#856),#627,.F.);
#4472=ADVANCED_FACE('',(#857),#4234,.F.);
#4473=ADVANCED_FACE('',(#858),#628,.F.);
#4474=ADVANCED_FACE('',(#859),#4235,.F.);
#4475=ADVANCED_FACE('',(#860),#629,.F.);
#4476=ADVANCED_FACE('',(#861),#4236,.F.);
#4477=ADVANCED_FACE('',(#862),#4237,.F.);
#4478=ADVANCED_FACE('',(#863),#4238,.F.);
#4479=ADVANCED_FACE('',(#864),#4239,.F.);
#4480=ADVANCED_FACE('',(#865),#4240,.F.);
#4481=ADVANCED_FACE('',(#866),#4241,.F.);
#4482=ADVANCED_FACE('',(#867),#4242,.F.);
#4483=ADVANCED_FACE('',(#868),#4243,.F.);
#4484=ADVANCED_FACE('',(#869,#441),#630,.T.);
#4485=ADVANCED_FACE('',(#870),#4244,.F.);
#4486=ADVANCED_FACE('',(#871,#442),#631,.F.);
#4487=ADVANCED_FACE('',(#872,#443,#444,#445,#446,#447,#448,#449,#450,#451,
#452,#453,#454,#455,#456,#457,#458,#459,#460,#461,#462,#463,#464,#465,#466,
#467),#632,.F.);
#4488=ADVANCED_FACE('',(#873),#4245,.F.);
#4489=ADVANCED_FACE('',(#874),#4246,.T.);
#4490=ADVANCED_FACE('',(#875,#468,#469,#470,#471,#472,#473,#474,#475,#476),
#633,.T.);
#4491=ADVANCED_FACE('',(#876),#4247,.F.);
#4492=ADVANCED_FACE('',(#877),#4248,.T.);
#4493=ADVANCED_FACE('',(#878,#477,#478,#479,#480,#481),#634,.F.);
#4494=ADVANCED_FACE('',(#879),#4249,.F.);
#4495=ADVANCED_FACE('',(#880),#4250,.T.);
#4496=ADVANCED_FACE('',(#881,#482),#635,.T.);
#4497=ADVANCED_FACE('',(#882,#483),#636,.F.);
#4498=ADVANCED_FACE('',(#883),#4251,.F.);
#4499=ADVANCED_FACE('',(#884),#4252,.F.);
#4500=ADVANCED_FACE('',(#885),#4253,.F.);
#4501=ADVANCED_FACE('',(#886),#4254,.F.);
#4502=ADVANCED_FACE('',(#887),#4255,.T.);
#4503=ADVANCED_FACE('',(#888,#484),#637,.T.);
#4504=ADVANCED_FACE('',(#889),#4256,.F.);
#4505=ADVANCED_FACE('',(#890),#4257,.T.);
#4506=ADVANCED_FACE('',(#891,#485,#486,#487,#488,#489),#638,.T.);
#4507=ADVANCED_FACE('',(#892,#490,#491,#492,#493,#494),#639,.F.);
#4508=ADVANCED_FACE('',(#893),#4258,.F.);
#4509=ADVANCED_FACE('',(#894),#4259,.F.);
#4510=ADVANCED_FACE('',(#895),#4260,.F.);
#4511=ADVANCED_FACE('',(#896),#4261,.F.);
#4512=ADVANCED_FACE('',(#897),#4262,.F.);
#4513=ADVANCED_FACE('',(#898),#4263,.F.);
#4514=ADVANCED_FACE('',(#899),#4264,.F.);
#4515=ADVANCED_FACE('',(#900),#4265,.F.);
#4516=ADVANCED_FACE('',(#901),#4266,.F.);
#4517=ADVANCED_FACE('',(#902),#4267,.F.);
#4518=ADVANCED_FACE('',(#903),#4268,.F.);
#4519=ADVANCED_FACE('',(#904),#4269,.F.);
#4520=ADVANCED_FACE('',(#905),#4270,.F.);
#4521=ADVANCED_FACE('',(#906),#4271,.F.);
#4522=ADVANCED_FACE('',(#907),#4272,.F.);
#4523=ADVANCED_FACE('',(#908),#4273,.F.);
#4524=ADVANCED_FACE('',(#909),#4274,.F.);
#4525=ADVANCED_FACE('',(#910),#4275,.T.);
#4526=ADVANCED_FACE('',(#911,#495,#496,#497,#498,#499,#500,#501,#502,#503,
#504,#505,#506,#507,#508,#509,#510,#511),#640,.T.);
#4527=ADVANCED_FACE('',(#912,#512,#513,#514,#515,#516,#517,#518,#519,#520,
#521,#522,#523,#524,#525,#526,#527,#528),#641,.F.);
#4528=ADVANCED_FACE('',(#913),#642,.T.);
#4529=ADVANCED_FACE('',(#914),#223,.T.);
#4530=ADVANCED_FACE('',(#915),#4276,.T.);
#4531=ADVANCED_FACE('',(#916),#224,.T.);
#4532=ADVANCED_FACE('',(#917,#529),#643,.T.);
#4533=ADVANCED_FACE('',(#918),#225,.T.);
#4534=ADVANCED_FACE('',(#919),#4277,.T.);
#4535=ADVANCED_FACE('',(#920),#226,.T.);
#4536=ADVANCED_FACE('',(#921),#644,.T.);
#4537=ADVANCED_FACE('',(#922),#645,.F.);
#4538=ADVANCED_FACE('',(#923),#646,.F.);
#4539=ADVANCED_FACE('',(#924),#647,.F.);
#4540=ADVANCED_FACE('',(#925),#648,.F.);
#4541=ADVANCED_FACE('',(#926),#649,.F.);
#4542=ADVANCED_FACE('',(#927),#650,.F.);
#4543=ADVANCED_FACE('',(#928),#651,.F.);
#4544=ADVANCED_FACE('',(#929),#652,.F.);
#4545=ADVANCED_FACE('',(#930),#653,.F.);
#4546=ADVANCED_FACE('',(#931,#530),#654,.T.);
#4547=ADVANCED_FACE('',(#932,#531),#655,.F.);
#4548=ADVANCED_FACE('',(#933),#4278,.T.);
#4549=ADVANCED_FACE('',(#934),#4279,.T.);
#4550=ADVANCED_FACE('',(#935),#4280,.T.);
#4551=ADVANCED_FACE('',(#936),#656,.T.);
#4552=ADVANCED_FACE('',(#937),#657,.T.);
#4553=ADVANCED_FACE('',(#938),#4281,.F.);
#4554=ADVANCED_FACE('',(#939),#658,.T.);
#4555=ADVANCED_FACE('',(#940,#532),#4282,.F.);
#4556=ADVANCED_FACE('',(#941,#533),#4283,.T.);
#4557=ADVANCED_FACE('',(#942,#534),#659,.T.);
#4558=ADVANCED_FACE('',(#943,#535),#660,.F.);
#4559=ADVANCED_FACE('',(#944),#661,.F.);
#4560=ADVANCED_FACE('',(#945),#662,.F.);
#4561=ADVANCED_FACE('',(#946),#663,.F.);
#4562=ADVANCED_FACE('',(#947),#664,.F.);
#4563=ADVANCED_FACE('',(#948),#665,.F.);
#4564=ADVANCED_FACE('',(#949),#666,.F.);
#4565=ADVANCED_FACE('',(#950),#667,.F.);
#4566=ADVANCED_FACE('',(#951,#536),#668,.T.);
#4567=ADVANCED_FACE('',(#952),#227,.T.);
#4568=ADVANCED_FACE('',(#953),#4284,.T.);
#4569=ADVANCED_FACE('',(#954),#228,.T.);
#4570=ADVANCED_FACE('',(#955),#669,.T.);
#4571=CLOSED_SHELL('',(#4285,#4286,#4287,#4288,#4289,#4290,#4291,#4292,
#4293,#4294,#4295,#4296,#4297));
#4572=CLOSED_SHELL('',(#4298,#4299,#4300));
#4573=CLOSED_SHELL('',(#4301,#4302,#4303));
#4574=CLOSED_SHELL('',(#4304,#4305,#4306));
#4575=CLOSED_SHELL('',(#4307,#4308,#4309));
#4576=CLOSED_SHELL('',(#4310,#4311,#4312,#4313,#4314,#4315,#4316,#4317,
#4318,#4319,#4320,#4321,#4322));
#4577=CLOSED_SHELL('',(#4323,#4324,#4325,#4326));
#4578=CLOSED_SHELL('',(#4327,#4328,#4329,#4330,#4331,#4332,#4333));
#4579=CLOSED_SHELL('',(#4334,#4335,#4336,#4337,#4338,#4339,#4340,#4341));
#4580=CLOSED_SHELL('',(#4342,#4343,#4344,#4345,#4346,#4347));
#4581=CLOSED_SHELL('',(#4348,#4349,#4350));
#4582=CLOSED_SHELL('',(#4351,#4352,#4353,#4354));
#4583=CLOSED_SHELL('',(#4355,#4356,#4357,#4358,#4359,#4360,#4361,#4362));
#4584=CLOSED_SHELL('',(#4363,#4364,#4365,#4366,#4367,#4368,#4369,#4370));
#4585=CLOSED_SHELL('',(#4371,#4372,#4373,#4374,#4375,#4376,#4377,#4378));
#4586=CLOSED_SHELL('',(#4379,#4380,#4381,#4382,#4383,#4384,#4385,#4386));
#4587=CLOSED_SHELL('',(#4387));
#4588=CLOSED_SHELL('',(#4388));
#4589=CLOSED_SHELL('',(#4389));
#4590=CLOSED_SHELL('',(#4390));
#4591=CLOSED_SHELL('',(#4391));
#4592=CLOSED_SHELL('',(#4392));
#4593=CLOSED_SHELL('',(#4393));
#4594=CLOSED_SHELL('',(#4394));
#4595=CLOSED_SHELL('',(#4395));
#4596=CLOSED_SHELL('',(#4396,#4397,#4398,#4399,#4400,#4401,#4402,#4403,
#4404,#4405,#4406,#4407,#4408,#4409,#4410,#4411,#4412,#4413,#4414,#4415,
#4416));
#4597=CLOSED_SHELL('',(#4417,#4418,#4419,#4420));
#4598=CLOSED_SHELL('',(#4421,#4422,#4423,#4424));
#4599=CLOSED_SHELL('',(#4425,#4426,#4427,#4428,#4429,#4430,#4431,#4432,
#4433,#4434,#4435));
#4600=CLOSED_SHELL('',(#4436,#4437,#4438,#4439,#4440,#4441,#4442,#4443,
#4444,#4445,#4446,#4447,#4448,#4449,#4450,#4451,#4452,#4453,#4454,#4455,
#4456,#4457,#4458,#4459,#4460,#4461,#4462,#4463,#4464,#4465,#4466,#4467,
#4468,#4469,#4470,#4471,#4472,#4473,#4474,#4475,#4476,#4477,#4478,#4479,
#4480,#4481,#4482,#4483,#4484,#4485,#4486,#4487,#4488,#4489,#4490,#4491,
#4492,#4493));
#4601=CLOSED_SHELL('',(#4494,#4495,#4496,#4497));
#4602=CLOSED_SHELL('',(#4498,#4499,#4500,#4501,#4502,#4503,#4504,#4505,
#4506,#4507));
#4603=CLOSED_SHELL('',(#4508,#4509,#4510,#4511,#4512,#4513,#4514,#4515,
#4516,#4517,#4518,#4519,#4520,#4521,#4522,#4523,#4524,#4525,#4526,#4527));
#4604=CLOSED_SHELL('',(#4528,#4529,#4530,#4531,#4532,#4533,#4534,#4535,
#4536));
#4605=CLOSED_SHELL('',(#4537,#4538,#4539,#4540,#4541,#4542,#4543,#4544));
#4606=CLOSED_SHELL('',(#4545,#4546,#4547,#4548,#4549,#4550,#4551));
#4607=CLOSED_SHELL('',(#4552,#4553,#4554,#4555,#4556,#4557,#4558));
#4608=CLOSED_SHELL('',(#4559,#4560,#4561,#4562,#4563,#4564,#4565,#4566,
#4567,#4568,#4569,#4570));
#4609=DERIVED_UNIT_ELEMENT(#4663,1.);
#4610=DERIVED_UNIT_ELEMENT(#10022,-3.);
#4611=DERIVED_UNIT_ELEMENT(#4663,1.);
#4612=DERIVED_UNIT_ELEMENT(#10022,-3.);
#4613=DERIVED_UNIT_ELEMENT(#4663,1.);
#4614=DERIVED_UNIT_ELEMENT(#10022,-3.);
#4615=DERIVED_UNIT_ELEMENT(#4663,1.);
#4616=DERIVED_UNIT_ELEMENT(#10022,-3.);
#4617=DERIVED_UNIT_ELEMENT(#4663,1.);
#4618=DERIVED_UNIT_ELEMENT(#10022,-3.);
#4619=DERIVED_UNIT_ELEMENT(#4663,1.);
#4620=DERIVED_UNIT_ELEMENT(#10022,-3.);
#4621=DERIVED_UNIT_ELEMENT(#4663,1.);
#4622=DERIVED_UNIT_ELEMENT(#10022,-3.);
#4623=DERIVED_UNIT_ELEMENT(#4663,1.);
#4624=DERIVED_UNIT_ELEMENT(#10022,-3.);
#4625=DERIVED_UNIT_ELEMENT(#4663,1.);
#4626=DERIVED_UNIT_ELEMENT(#10022,-3.);
#4627=DERIVED_UNIT_ELEMENT(#4663,1.);
#4628=DERIVED_UNIT_ELEMENT(#10022,-3.);
#4629=DERIVED_UNIT_ELEMENT(#4663,1.);
#4630=DERIVED_UNIT_ELEMENT(#10022,-3.);
#4631=DERIVED_UNIT_ELEMENT(#4663,1.);
#4632=DERIVED_UNIT_ELEMENT(#10022,-3.);
#4633=DERIVED_UNIT_ELEMENT(#4663,1.);
#4634=DERIVED_UNIT_ELEMENT(#10022,-3.);
#4635=DERIVED_UNIT_ELEMENT(#4663,1.);
#4636=DERIVED_UNIT_ELEMENT(#10022,-3.);
#4637=DERIVED_UNIT_ELEMENT(#4663,1.);
#4638=DERIVED_UNIT_ELEMENT(#10022,-3.);
#4639=DERIVED_UNIT_ELEMENT(#4663,1.);
#4640=DERIVED_UNIT_ELEMENT(#10022,-3.);
#4641=DERIVED_UNIT_ELEMENT(#4663,1.);
#4642=DERIVED_UNIT_ELEMENT(#10022,-3.);
#4643=DERIVED_UNIT_ELEMENT(#4663,1.);
#4644=DERIVED_UNIT_ELEMENT(#10022,-3.);
#4645=DERIVED_UNIT_ELEMENT(#4663,1.);
#4646=DERIVED_UNIT_ELEMENT(#10022,-3.);
#4647=DERIVED_UNIT_ELEMENT(#4663,1.);
#4648=DERIVED_UNIT_ELEMENT(#10022,-3.);
#4649=DERIVED_UNIT_ELEMENT(#4663,1.);
#4650=DERIVED_UNIT_ELEMENT(#10022,-3.);
#4651=DERIVED_UNIT_ELEMENT(#4663,1.);
#4652=DERIVED_UNIT_ELEMENT(#10022,-3.);
#4653=DERIVED_UNIT_ELEMENT(#4663,1.);
#4654=DERIVED_UNIT_ELEMENT(#10022,-3.);
#4655=DERIVED_UNIT_ELEMENT(#4663,1.);
#4656=DERIVED_UNIT_ELEMENT(#10022,-3.);
#4657=DERIVED_UNIT_ELEMENT(#4663,1.);
#4658=DERIVED_UNIT_ELEMENT(#10022,-3.);
#4659=DERIVED_UNIT_ELEMENT(#4663,1.);
#4660=DERIVED_UNIT_ELEMENT(#10022,-3.);
#4661=DERIVED_UNIT_ELEMENT(#4663,1.);
#4662=DERIVED_UNIT_ELEMENT(#10022,-3.);
#4663=(
MASS_UNIT()
NAMED_UNIT(*)
SI_UNIT(.KILO.,.GRAM.)
);
#4664=DERIVED_UNIT((#4609,#4610));
#4665=DERIVED_UNIT((#4611,#4612));
#4666=DERIVED_UNIT((#4613,#4614));
#4667=DERIVED_UNIT((#4615,#4616));
#4668=DERIVED_UNIT((#4617,#4618));
#4669=DERIVED_UNIT((#4619,#4620));
#4670=DERIVED_UNIT((#4621,#4622));
#4671=DERIVED_UNIT((#4623,#4624));
#4672=DERIVED_UNIT((#4625,#4626));
#4673=DERIVED_UNIT((#4627,#4628));
#4674=DERIVED_UNIT((#4629,#4630));
#4675=DERIVED_UNIT((#4631,#4632));
#4676=DERIVED_UNIT((#4633,#4634));
#4677=DERIVED_UNIT((#4635,#4636));
#4678=DERIVED_UNIT((#4637,#4638));
#4679=DERIVED_UNIT((#4639,#4640));
#4680=DERIVED_UNIT((#4641,#4642));
#4681=DERIVED_UNIT((#4643,#4644));
#4682=DERIVED_UNIT((#4645,#4646));
#4683=DERIVED_UNIT((#4647,#4648));
#4684=DERIVED_UNIT((#4649,#4650));
#4685=DERIVED_UNIT((#4651,#4652));
#4686=DERIVED_UNIT((#4653,#4654));
#4687=DERIVED_UNIT((#4655,#4656));
#4688=DERIVED_UNIT((#4657,#4658));
#4689=DERIVED_UNIT((#4659,#4660));
#4690=DERIVED_UNIT((#4661,#4662));
#4691=MEASURE_REPRESENTATION_ITEM('density measure',
POSITIVE_RATIO_MEASURE(7850.),#4664);
#4692=MEASURE_REPRESENTATION_ITEM('density measure',
POSITIVE_RATIO_MEASURE(7850.),#4665);
#4693=MEASURE_REPRESENTATION_ITEM('density measure',
POSITIVE_RATIO_MEASURE(7850.),#4666);
#4694=MEASURE_REPRESENTATION_ITEM('density measure',
POSITIVE_RATIO_MEASURE(7850.),#4667);
#4695=MEASURE_REPRESENTATION_ITEM('density measure',
POSITIVE_RATIO_MEASURE(7850.),#4668);
#4696=MEASURE_REPRESENTATION_ITEM('density measure',
POSITIVE_RATIO_MEASURE(7850.),#4669);
#4697=MEASURE_REPRESENTATION_ITEM('density measure',
POSITIVE_RATIO_MEASURE(7850.),#4670);
#4698=MEASURE_REPRESENTATION_ITEM('density measure',
POSITIVE_RATIO_MEASURE(7850.),#4671);
#4699=MEASURE_REPRESENTATION_ITEM('density measure',
POSITIVE_RATIO_MEASURE(7850.),#4672);
#4700=MEASURE_REPRESENTATION_ITEM('density measure',
POSITIVE_RATIO_MEASURE(7850.),#4673);
#4701=MEASURE_REPRESENTATION_ITEM('density measure',
POSITIVE_RATIO_MEASURE(7850.),#4674);
#4702=MEASURE_REPRESENTATION_ITEM('density measure',
POSITIVE_RATIO_MEASURE(7850.),#4675);
#4703=MEASURE_REPRESENTATION_ITEM('density measure',
POSITIVE_RATIO_MEASURE(7850.),#4676);
#4704=MEASURE_REPRESENTATION_ITEM('density measure',
POSITIVE_RATIO_MEASURE(7850.),#4677);
#4705=MEASURE_REPRESENTATION_ITEM('density measure',
POSITIVE_RATIO_MEASURE(7850.),#4678);
#4706=MEASURE_REPRESENTATION_ITEM('density measure',
POSITIVE_RATIO_MEASURE(7850.),#4679);
#4707=MEASURE_REPRESENTATION_ITEM('density measure',
POSITIVE_RATIO_MEASURE(7850.),#4680);
#4708=MEASURE_REPRESENTATION_ITEM('density measure',
POSITIVE_RATIO_MEASURE(7850.),#4681);
#4709=MEASURE_REPRESENTATION_ITEM('density measure',
POSITIVE_RATIO_MEASURE(7850.),#4682);
#4710=MEASURE_REPRESENTATION_ITEM('density measure',
POSITIVE_RATIO_MEASURE(7850.),#4683);
#4711=MEASURE_REPRESENTATION_ITEM('density measure',
POSITIVE_RATIO_MEASURE(7850.),#4684);
#4712=MEASURE_REPRESENTATION_ITEM('density measure',
POSITIVE_RATIO_MEASURE(7850.),#4685);
#4713=MEASURE_REPRESENTATION_ITEM('density measure',
POSITIVE_RATIO_MEASURE(7850.),#4686);
#4714=MEASURE_REPRESENTATION_ITEM('density measure',
POSITIVE_RATIO_MEASURE(7850.),#4687);
#4715=MEASURE_REPRESENTATION_ITEM('density measure',
POSITIVE_RATIO_MEASURE(7850.),#4688);
#4716=MEASURE_REPRESENTATION_ITEM('density measure',
POSITIVE_RATIO_MEASURE(7850.),#4689);
#4717=MEASURE_REPRESENTATION_ITEM('density measure',
POSITIVE_RATIO_MEASURE(7850.),#4690);
#4718=PROPERTY_DEFINITION_REPRESENTATION(#4853,#4772);
#4719=PROPERTY_DEFINITION_REPRESENTATION(#4854,#4773);
#4720=PROPERTY_DEFINITION_REPRESENTATION(#4855,#4774);
#4721=PROPERTY_DEFINITION_REPRESENTATION(#4856,#4775);
#4722=PROPERTY_DEFINITION_REPRESENTATION(#4857,#4776);
#4723=PROPERTY_DEFINITION_REPRESENTATION(#4858,#4777);
#4724=PROPERTY_DEFINITION_REPRESENTATION(#4859,#4778);
#4725=PROPERTY_DEFINITION_REPRESENTATION(#4860,#4779);
#4726=PROPERTY_DEFINITION_REPRESENTATION(#4861,#4780);
#4727=PROPERTY_DEFINITION_REPRESENTATION(#4862,#4781);
#4728=PROPERTY_DEFINITION_REPRESENTATION(#4863,#4782);
#4729=PROPERTY_DEFINITION_REPRESENTATION(#4864,#4783);
#4730=PROPERTY_DEFINITION_REPRESENTATION(#4865,#4784);
#4731=PROPERTY_DEFINITION_REPRESENTATION(#4866,#4785);
#4732=PROPERTY_DEFINITION_REPRESENTATION(#4867,#4786);
#4733=PROPERTY_DEFINITION_REPRESENTATION(#4868,#4787);
#4734=PROPERTY_DEFINITION_REPRESENTATION(#4869,#4788);
#4735=PROPERTY_DEFINITION_REPRESENTATION(#4870,#4789);
#4736=PROPERTY_DEFINITION_REPRESENTATION(#4871,#4790);
#4737=PROPERTY_DEFINITION_REPRESENTATION(#4872,#4791);
#4738=PROPERTY_DEFINITION_REPRESENTATION(#4873,#4792);
#4739=PROPERTY_DEFINITION_REPRESENTATION(#4874,#4793);
#4740=PROPERTY_DEFINITION_REPRESENTATION(#4875,#4794);
#4741=PROPERTY_DEFINITION_REPRESENTATION(#4876,#4795);
#4742=PROPERTY_DEFINITION_REPRESENTATION(#4877,#4796);
#4743=PROPERTY_DEFINITION_REPRESENTATION(#4878,#4797);
#4744=PROPERTY_DEFINITION_REPRESENTATION(#4879,#4798);
#4745=PROPERTY_DEFINITION_REPRESENTATION(#4880,#4799);
#4746=PROPERTY_DEFINITION_REPRESENTATION(#4881,#4800);
#4747=PROPERTY_DEFINITION_REPRESENTATION(#4882,#4801);
#4748=PROPERTY_DEFINITION_REPRESENTATION(#4883,#4802);
#4749=PROPERTY_DEFINITION_REPRESENTATION(#4884,#4803);
#4750=PROPERTY_DEFINITION_REPRESENTATION(#4885,#4804);
#4751=PROPERTY_DEFINITION_REPRESENTATION(#4886,#4805);
#4752=PROPERTY_DEFINITION_REPRESENTATION(#4887,#4806);
#4753=PROPERTY_DEFINITION_REPRESENTATION(#4888,#4807);
#4754=PROPERTY_DEFINITION_REPRESENTATION(#4889,#4808);
#4755=PROPERTY_DEFINITION_REPRESENTATION(#4890,#4809);
#4756=PROPERTY_DEFINITION_REPRESENTATION(#4891,#4810);
#4757=PROPERTY_DEFINITION_REPRESENTATION(#4892,#4811);
#4758=PROPERTY_DEFINITION_REPRESENTATION(#4893,#4812);
#4759=PROPERTY_DEFINITION_REPRESENTATION(#4894,#4813);
#4760=PROPERTY_DEFINITION_REPRESENTATION(#4895,#4814);
#4761=PROPERTY_DEFINITION_REPRESENTATION(#4896,#4815);
#4762=PROPERTY_DEFINITION_REPRESENTATION(#4897,#4816);
#4763=PROPERTY_DEFINITION_REPRESENTATION(#4898,#4817);
#4764=PROPERTY_DEFINITION_REPRESENTATION(#4899,#4818);
#4765=PROPERTY_DEFINITION_REPRESENTATION(#4900,#4819);
#4766=PROPERTY_DEFINITION_REPRESENTATION(#4901,#4820);
#4767=PROPERTY_DEFINITION_REPRESENTATION(#4902,#4821);
#4768=PROPERTY_DEFINITION_REPRESENTATION(#4903,#4822);
#4769=PROPERTY_DEFINITION_REPRESENTATION(#4904,#4823);
#4770=PROPERTY_DEFINITION_REPRESENTATION(#4905,#4824);
#4771=PROPERTY_DEFINITION_REPRESENTATION(#4906,#4825);
#4772=REPRESENTATION('material name',(#4826),#9990);
#4773=REPRESENTATION('density',(#4691),#9990);
#4774=REPRESENTATION('material name',(#4827),#9991);
#4775=REPRESENTATION('density',(#4692),#9991);
#4776=REPRESENTATION('material name',(#4828),#9992);
#4777=REPRESENTATION('density',(#4693),#9992);
#4778=REPRESENTATION('material name',(#4829),#9993);
#4779=REPRESENTATION('density',(#4694),#9993);
#4780=REPRESENTATION('material name',(#4830),#9994);
#4781=REPRESENTATION('density',(#4695),#9994);
#4782=REPRESENTATION('material name',(#4831),#9995);
#4783=REPRESENTATION('density',(#4696),#9995);
#4784=REPRESENTATION('material name',(#4832),#9996);
#4785=REPRESENTATION('density',(#4697),#9996);
#4786=REPRESENTATION('material name',(#4833),#9997);
#4787=REPRESENTATION('density',(#4698),#9997);
#4788=REPRESENTATION('material name',(#4834),#9998);
#4789=REPRESENTATION('density',(#4699),#9998);
#4790=REPRESENTATION('material name',(#4835),#9999);
#4791=REPRESENTATION('density',(#4700),#9999);
#4792=REPRESENTATION('material name',(#4836),#10000);
#4793=REPRESENTATION('density',(#4701),#10000);
#4794=REPRESENTATION('material name',(#4837),#10001);
#4795=REPRESENTATION('density',(#4702),#10001);
#4796=REPRESENTATION('material name',(#4838),#10002);
#4797=REPRESENTATION('density',(#4703),#10002);
#4798=REPRESENTATION('material name',(#4839),#10004);
#4799=REPRESENTATION('density',(#4704),#10004);
#4800=REPRESENTATION('material name',(#4840),#10005);
#4801=REPRESENTATION('density',(#4705),#10005);
#4802=REPRESENTATION('material name',(#4841),#10006);
#4803=REPRESENTATION('density',(#4706),#10006);
#4804=REPRESENTATION('material name',(#4842),#10007);
#4805=REPRESENTATION('density',(#4707),#10007);
#4806=REPRESENTATION('material name',(#4843),#10008);
#4807=REPRESENTATION('density',(#4708),#10008);
#4808=REPRESENTATION('material name',(#4844),#10009);
#4809=REPRESENTATION('density',(#4709),#10009);
#4810=REPRESENTATION('material name',(#4845),#10011);
#4811=REPRESENTATION('density',(#4710),#10011);
#4812=REPRESENTATION('material name',(#4846),#10012);
#4813=REPRESENTATION('density',(#4711),#10012);
#4814=REPRESENTATION('material name',(#4847),#10013);
#4815=REPRESENTATION('density',(#4712),#10013);
#4816=REPRESENTATION('material name',(#4848),#10014);
#4817=REPRESENTATION('density',(#4713),#10014);
#4818=REPRESENTATION('material name',(#4849),#10015);
#4819=REPRESENTATION('density',(#4714),#10015);
#4820=REPRESENTATION('material name',(#4850),#10017);
#4821=REPRESENTATION('density',(#4715),#10017);
#4822=REPRESENTATION('material name',(#4851),#10018);
#4823=REPRESENTATION('density',(#4716),#10018);
#4824=REPRESENTATION('material name',(#4852),#10019);
#4825=REPRESENTATION('density',(#4717),#10019);
#4826=DESCRIPTIVE_REPRESENTATION_ITEM('Steel','Steel');
#4827=DESCRIPTIVE_REPRESENTATION_ITEM('Steel','Steel');
#4828=DESCRIPTIVE_REPRESENTATION_ITEM('Steel','Steel');
#4829=DESCRIPTIVE_REPRESENTATION_ITEM('Steel','Steel');
#4830=DESCRIPTIVE_REPRESENTATION_ITEM('Steel','Steel');
#4831=DESCRIPTIVE_REPRESENTATION_ITEM('Steel','Steel');
#4832=DESCRIPTIVE_REPRESENTATION_ITEM('Steel','Steel');
#4833=DESCRIPTIVE_REPRESENTATION_ITEM('Steel','Steel');
#4834=DESCRIPTIVE_REPRESENTATION_ITEM('Steel','Steel');
#4835=DESCRIPTIVE_REPRESENTATION_ITEM('Steel','Steel');
#4836=DESCRIPTIVE_REPRESENTATION_ITEM('Steel','Steel');
#4837=DESCRIPTIVE_REPRESENTATION_ITEM('Steel','Steel');
#4838=DESCRIPTIVE_REPRESENTATION_ITEM('Steel','Steel');
#4839=DESCRIPTIVE_REPRESENTATION_ITEM('Steel','Steel');
#4840=DESCRIPTIVE_REPRESENTATION_ITEM('Steel','Steel');
#4841=DESCRIPTIVE_REPRESENTATION_ITEM('Steel','Steel');
#4842=DESCRIPTIVE_REPRESENTATION_ITEM('Steel','Steel');
#4843=DESCRIPTIVE_REPRESENTATION_ITEM('Steel','Steel');
#4844=DESCRIPTIVE_REPRESENTATION_ITEM('Steel','Steel');
#4845=DESCRIPTIVE_REPRESENTATION_ITEM('Steel','Steel');
#4846=DESCRIPTIVE_REPRESENTATION_ITEM('Steel','Steel');
#4847=DESCRIPTIVE_REPRESENTATION_ITEM('Steel','Steel');
#4848=DESCRIPTIVE_REPRESENTATION_ITEM('Steel','Steel');
#4849=DESCRIPTIVE_REPRESENTATION_ITEM('Steel','Steel');
#4850=DESCRIPTIVE_REPRESENTATION_ITEM('Steel','Steel');
#4851=DESCRIPTIVE_REPRESENTATION_ITEM('Steel','Steel');
#4852=DESCRIPTIVE_REPRESENTATION_ITEM('Steel','Steel');
#4853=PROPERTY_DEFINITION('material property','material name',#10170);
#4854=PROPERTY_DEFINITION('material property','density of part',#10170);
#4855=PROPERTY_DEFINITION('material property','material name',#10171);
#4856=PROPERTY_DEFINITION('material property','density of part',#10171);
#4857=PROPERTY_DEFINITION('material property','material name',#10172);
#4858=PROPERTY_DEFINITION('material property','density of part',#10172);
#4859=PROPERTY_DEFINITION('material property','material name',#10173);
#4860=PROPERTY_DEFINITION('material property','density of part',#10173);
#4861=PROPERTY_DEFINITION('material property','material name',#10174);
#4862=PROPERTY_DEFINITION('material property','density of part',#10174);
#4863=PROPERTY_DEFINITION('material property','material name',#10175);
#4864=PROPERTY_DEFINITION('material property','density of part',#10175);
#4865=PROPERTY_DEFINITION('material property','material name',#10176);
#4866=PROPERTY_DEFINITION('material property','density of part',#10176);
#4867=PROPERTY_DEFINITION('material property','material name',#10177);
#4868=PROPERTY_DEFINITION('material property','density of part',#10177);
#4869=PROPERTY_DEFINITION('material property','material name',#10178);
#4870=PROPERTY_DEFINITION('material property','density of part',#10178);
#4871=PROPERTY_DEFINITION('material property','material name',#10179);
#4872=PROPERTY_DEFINITION('material property','density of part',#10179);
#4873=PROPERTY_DEFINITION('material property','material name',#10180);
#4874=PROPERTY_DEFINITION('material property','density of part',#10180);
#4875=PROPERTY_DEFINITION('material property','material name',#10181);
#4876=PROPERTY_DEFINITION('material property','density of part',#10181);
#4877=PROPERTY_DEFINITION('material property','material name',#10182);
#4878=PROPERTY_DEFINITION('material property','density of part',#10182);
#4879=PROPERTY_DEFINITION('material property','material name',#10184);
#4880=PROPERTY_DEFINITION('material property','density of part',#10184);
#4881=PROPERTY_DEFINITION('material property','material name',#10185);
#4882=PROPERTY_DEFINITION('material property','density of part',#10185);
#4883=PROPERTY_DEFINITION('material property','material name',#10186);
#4884=PROPERTY_DEFINITION('material property','density of part',#10186);
#4885=PROPERTY_DEFINITION('material property','material name',#10187);
#4886=PROPERTY_DEFINITION('material property','density of part',#10187);
#4887=PROPERTY_DEFINITION('material property','material name',#10188);
#4888=PROPERTY_DEFINITION('material property','density of part',#10188);
#4889=PROPERTY_DEFINITION('material property','material name',#10189);
#4890=PROPERTY_DEFINITION('material property','density of part',#10189);
#4891=PROPERTY_DEFINITION('material property','material name',#10191);
#4892=PROPERTY_DEFINITION('material property','density of part',#10191);
#4893=PROPERTY_DEFINITION('material property','material name',#10192);
#4894=PROPERTY_DEFINITION('material property','density of part',#10192);
#4895=PROPERTY_DEFINITION('material property','material name',#10193);
#4896=PROPERTY_DEFINITION('material property','density of part',#10193);
#4897=PROPERTY_DEFINITION('material property','material name',#10194);
#4898=PROPERTY_DEFINITION('material property','density of part',#10194);
#4899=PROPERTY_DEFINITION('material property','material name',#10195);
#4900=PROPERTY_DEFINITION('material property','density of part',#10195);
#4901=PROPERTY_DEFINITION('material property','material name',#10197);
#4902=PROPERTY_DEFINITION('material property','density of part',#10197);
#4903=PROPERTY_DEFINITION('material property','material name',#10198);
#4904=PROPERTY_DEFINITION('material property','density of part',#10198);
#4905=PROPERTY_DEFINITION('material property','material name',#10199);
#4906=PROPERTY_DEFINITION('material property','density of part',#10199);
#4907=AXIS2_PLACEMENT_3D('',#7125,#5573,#5574);
#4908=AXIS2_PLACEMENT_3D('',#7126,#5575,#5576);
#4909=AXIS2_PLACEMENT_3D('',#7127,#5577,#5578);
#4910=AXIS2_PLACEMENT_3D('',#7128,#5579,#5580);
#4911=AXIS2_PLACEMENT_3D('',#7130,#5581,#5582);
#4912=AXIS2_PLACEMENT_3D('',#7133,#5584,#5585);
#4913=AXIS2_PLACEMENT_3D('',#7134,#5586,#5587);
#4914=AXIS2_PLACEMENT_3D('',#7136,#5588,#5589);
#4915=AXIS2_PLACEMENT_3D('',#7139,#5591,#5592);
#4916=AXIS2_PLACEMENT_3D('',#7140,#5593,#5594);
#4917=AXIS2_PLACEMENT_3D('',#7142,#5595,#5596);
#4918=AXIS2_PLACEMENT_3D('',#7145,#5598,#5599);
#4919=AXIS2_PLACEMENT_3D('',#7146,#5600,#5601);
#4920=AXIS2_PLACEMENT_3D('',#7148,#5602,#5603);
#4921=AXIS2_PLACEMENT_3D('',#7151,#5605,#5606);
#4922=AXIS2_PLACEMENT_3D('',#7152,#5607,#5608);
#4923=AXIS2_PLACEMENT_3D('',#7154,#5609,#5610);
#4924=AXIS2_PLACEMENT_3D('',#7157,#5612,#5613);
#4925=AXIS2_PLACEMENT_3D('',#7158,#5614,#5615);
#4926=AXIS2_PLACEMENT_3D('',#7160,#5616,#5617);
#4927=AXIS2_PLACEMENT_3D('',#7163,#5619,#5620);
#4928=AXIS2_PLACEMENT_3D('',#7164,#5621,#5622);
#4929=AXIS2_PLACEMENT_3D('',#7166,#5623,#5624);
#4930=AXIS2_PLACEMENT_3D('',#7169,#5626,#5627);
#4931=AXIS2_PLACEMENT_3D('',#7170,#5628,#5629);
#4932=AXIS2_PLACEMENT_3D('',#7179,#5634,#5635);
#4933=AXIS2_PLACEMENT_3D('',#7185,#5639,#5640);
#4934=AXIS2_PLACEMENT_3D('',#7191,#5644,#5645);
#4935=AXIS2_PLACEMENT_3D('',#7194,#5648,#5649);
#4936=AXIS2_PLACEMENT_3D('',#7195,#5650,#5651);
#4937=AXIS2_PLACEMENT_3D('',#7196,#5652,#5653);
#4938=AXIS2_PLACEMENT_3D('',#7197,#5654,#5655);
#4939=AXIS2_PLACEMENT_3D('',#7199,#5656,#5657);
#4940=AXIS2_PLACEMENT_3D('',#7202,#5659,#5660);
#4941=AXIS2_PLACEMENT_3D('',#7203,#5661,#5662);
#4942=AXIS2_PLACEMENT_3D('',#7204,#5663,#5664);
#4943=AXIS2_PLACEMENT_3D('',#7205,#5665,#5666);
#4944=AXIS2_PLACEMENT_3D('',#7206,#5667,#5668);
#4945=AXIS2_PLACEMENT_3D('',#7208,#5669,#5670);
#4946=AXIS2_PLACEMENT_3D('',#7211,#5672,#5673);
#4947=AXIS2_PLACEMENT_3D('',#7212,#5674,#5675);
#4948=AXIS2_PLACEMENT_3D('',#7213,#5676,#5677);
#4949=AXIS2_PLACEMENT_3D('',#7214,#5678,#5679);
#4950=AXIS2_PLACEMENT_3D('',#7215,#5680,#5681);
#4951=AXIS2_PLACEMENT_3D('',#7217,#5682,#5683);
#4952=AXIS2_PLACEMENT_3D('',#7220,#5685,#5686);
#4953=AXIS2_PLACEMENT_3D('',#7221,#5687,#5688);
#4954=AXIS2_PLACEMENT_3D('',#7222,#5689,#5690);
#4955=AXIS2_PLACEMENT_3D('',#7223,#5691,#5692);
#4956=AXIS2_PLACEMENT_3D('',#7224,#5693,#5694);
#4957=AXIS2_PLACEMENT_3D('',#7226,#5695,#5696);
#4958=AXIS2_PLACEMENT_3D('',#7229,#5698,#5699);
#4959=AXIS2_PLACEMENT_3D('',#7230,#5700,#5701);
#4960=AXIS2_PLACEMENT_3D('',#7231,#5702,#5703);
#4961=AXIS2_PLACEMENT_3D('',#7232,#5704,#5705);
#4962=AXIS2_PLACEMENT_3D('',#7233,#5706,#5707);
#4963=AXIS2_PLACEMENT_3D('',#7235,#5708,#5709);
#4964=AXIS2_PLACEMENT_3D('',#7238,#5711,#5712);
#4965=AXIS2_PLACEMENT_3D('',#7239,#5713,#5714);
#4966=AXIS2_PLACEMENT_3D('',#7241,#5715,#5716);
#4967=AXIS2_PLACEMENT_3D('',#7244,#5718,#5719);
#4968=AXIS2_PLACEMENT_3D('',#7245,#5720,#5721);
#4969=AXIS2_PLACEMENT_3D('',#7247,#5722,#5723);
#4970=AXIS2_PLACEMENT_3D('',#7250,#5725,#5726);
#4971=AXIS2_PLACEMENT_3D('',#7251,#5727,#5728);
#4972=AXIS2_PLACEMENT_3D('',#7253,#5729,#5730);
#4973=AXIS2_PLACEMENT_3D('',#7256,#5732,#5733);
#4974=AXIS2_PLACEMENT_3D('',#7257,#5734,#5735);
#4975=AXIS2_PLACEMENT_3D('',#7259,#5736,#5737);
#4976=AXIS2_PLACEMENT_3D('',#7261,#5738,#5739);
#4977=AXIS2_PLACEMENT_3D('',#7262,#5740,#5741);
#4978=AXIS2_PLACEMENT_3D('',#7264,#5742,#5743);
#4979=AXIS2_PLACEMENT_3D('',#7266,#5744,#5745);
#4980=AXIS2_PLACEMENT_3D('',#7267,#5746,#5747);
#4981=AXIS2_PLACEMENT_3D('',#7269,#5749,#5750);
#4982=AXIS2_PLACEMENT_3D('',#7272,#5752,#5753);
#4983=AXIS2_PLACEMENT_3D('',#7273,#5754,#5755);
#4984=AXIS2_PLACEMENT_3D('',#7275,#5756,#5757);
#4985=AXIS2_PLACEMENT_3D('',#7276,#5758,#5759);
#4986=AXIS2_PLACEMENT_3D('',#7279,#5761,#5762);
#4987=AXIS2_PLACEMENT_3D('',#7280,#5763,#5764);
#4988=AXIS2_PLACEMENT_3D('',#7282,#5765,#5766);
#4989=AXIS2_PLACEMENT_3D('',#7284,#5768,#5769);
#4990=AXIS2_PLACEMENT_3D('',#7285,#5770,#5771);
#4991=AXIS2_PLACEMENT_3D('',#7286,#5772,#5773);
#4992=AXIS2_PLACEMENT_3D('',#7287,#5774,#5775);
#4993=AXIS2_PLACEMENT_3D('',#7289,#5776,#5777);
#4994=AXIS2_PLACEMENT_3D('',#7292,#5779,#5780);
#4995=AXIS2_PLACEMENT_3D('',#7293,#5781,#5782);
#4996=AXIS2_PLACEMENT_3D('',#7295,#5783,#5784);
#4997=AXIS2_PLACEMENT_3D('',#7298,#5786,#5787);
#4998=AXIS2_PLACEMENT_3D('',#7299,#5788,#5789);
#4999=AXIS2_PLACEMENT_3D('',#7300,#5790,#5791);
#5000=AXIS2_PLACEMENT_3D('',#7301,#5792,#5793);
#5001=AXIS2_PLACEMENT_3D('',#7302,#5794,#5795);
#5002=AXIS2_PLACEMENT_3D('',#7306,#5797,#5798);
#5003=AXIS2_PLACEMENT_3D('',#7307,#5799,#5800);
#5004=AXIS2_PLACEMENT_3D('',#7324,#5801,#5802);
#5005=AXIS2_PLACEMENT_3D('',#7381,#5804,#5805);
#5006=AXIS2_PLACEMENT_3D('',#7383,#5807,#5808);
#5007=AXIS2_PLACEMENT_3D('',#7385,#5809,#5810);
#5008=AXIS2_PLACEMENT_3D('',#7388,#5812,#5813);
#5009=AXIS2_PLACEMENT_3D('',#7389,#5814,#5815);
#5010=AXIS2_PLACEMENT_3D('',#7391,#5816,#5817);
#5011=AXIS2_PLACEMENT_3D('',#7394,#5819,#5820);
#5012=AXIS2_PLACEMENT_3D('',#7395,#5821,#5822);
#5013=AXIS2_PLACEMENT_3D('',#7396,#5823,#5824);
#5014=AXIS2_PLACEMENT_3D('',#7397,#5825,#5826);
#5015=AXIS2_PLACEMENT_3D('',#7398,#5827,#5828);
#5016=AXIS2_PLACEMENT_3D('',#7400,#5829,#5830);
#5017=AXIS2_PLACEMENT_3D('',#7403,#5832,#5833);
#5018=AXIS2_PLACEMENT_3D('',#7404,#5834,#5835);
#5019=AXIS2_PLACEMENT_3D('',#7406,#5836,#5837);
#5020=AXIS2_PLACEMENT_3D('',#7409,#5839,#5840);
#5021=AXIS2_PLACEMENT_3D('',#7410,#5841,#5842);
#5022=AXIS2_PLACEMENT_3D('',#7412,#5843,#5844);
#5023=AXIS2_PLACEMENT_3D('',#7415,#5846,#5847);
#5024=AXIS2_PLACEMENT_3D('',#7416,#5848,#5849);
#5025=AXIS2_PLACEMENT_3D('',#7418,#5850,#5851);
#5026=AXIS2_PLACEMENT_3D('',#7419,#5852,#5853);
#5027=AXIS2_PLACEMENT_3D('',#7422,#5855,#5856);
#5028=AXIS2_PLACEMENT_3D('',#7423,#5857,#5858);
#5029=AXIS2_PLACEMENT_3D('',#7425,#5859,#5860);
#5030=AXIS2_PLACEMENT_3D('',#7428,#5862,#5863);
#5031=AXIS2_PLACEMENT_3D('',#7429,#5864,#5865);
#5032=AXIS2_PLACEMENT_3D('',#7430,#5866,#5867);
#5033=AXIS2_PLACEMENT_3D('',#7431,#5868,#5869);
#5034=AXIS2_PLACEMENT_3D('',#7432,#5870,#5871);
#5035=AXIS2_PLACEMENT_3D('',#7434,#5872,#5873);
#5036=AXIS2_PLACEMENT_3D('',#7437,#5875,#5876);
#5037=AXIS2_PLACEMENT_3D('',#7438,#5877,#5878);
#5038=AXIS2_PLACEMENT_3D('',#7440,#5879,#5880);
#5039=AXIS2_PLACEMENT_3D('',#7441,#5881,#5882);
#5040=AXIS2_PLACEMENT_3D('',#7444,#5884,#5885);
#5041=AXIS2_PLACEMENT_3D('',#7445,#5886,#5887);
#5042=AXIS2_PLACEMENT_3D('',#7447,#5888,#5889);
#5043=AXIS2_PLACEMENT_3D('',#7450,#5891,#5892);
#5044=AXIS2_PLACEMENT_3D('',#7451,#5893,#5894);
#5045=AXIS2_PLACEMENT_3D('',#7452,#5895,#5896);
#5046=AXIS2_PLACEMENT_3D('',#7453,#5897,#5898);
#5047=AXIS2_PLACEMENT_3D('',#8415,#5899,#5900);
#5048=AXIS2_PLACEMENT_3D('',#8513,#5901,#5902);
#5049=AXIS2_PLACEMENT_3D('',#8514,#5903,#5904);
#5050=AXIS2_PLACEMENT_3D('',#8515,#5905,#5906);
#5051=AXIS2_PLACEMENT_3D('',#8516,#5907,#5908);
#5052=AXIS2_PLACEMENT_3D('',#8517,#5909,#5910);
#5053=AXIS2_PLACEMENT_3D('',#8519,#5911,#5912);
#5054=AXIS2_PLACEMENT_3D('',#8522,#5914,#5915);
#5055=AXIS2_PLACEMENT_3D('',#8523,#5916,#5917);
#5056=AXIS2_PLACEMENT_3D('',#8525,#5918,#5919);
#5057=AXIS2_PLACEMENT_3D('',#8528,#5921,#5922);
#5058=AXIS2_PLACEMENT_3D('',#8529,#5923,#5924);
#5059=AXIS2_PLACEMENT_3D('',#8530,#5925,#5926);
#5060=AXIS2_PLACEMENT_3D('',#8531,#5927,#5928);
#5061=AXIS2_PLACEMENT_3D('',#8532,#5929,#5930);
#5062=AXIS2_PLACEMENT_3D('',#8541,#5935,#5936);
#5063=AXIS2_PLACEMENT_3D('',#8547,#5940,#5941);
#5064=AXIS2_PLACEMENT_3D('',#8553,#5945,#5946);
#5065=AXIS2_PLACEMENT_3D('',#8559,#5950,#5951);
#5066=AXIS2_PLACEMENT_3D('',#8565,#5955,#5956);
#5067=AXIS2_PLACEMENT_3D('',#8568,#5959,#5960);
#5068=AXIS2_PLACEMENT_3D('',#8569,#5961,#5962);
#5069=AXIS2_PLACEMENT_3D('',#8570,#5963,#5964);
#5070=AXIS2_PLACEMENT_3D('',#8572,#5965,#5966);
#5071=AXIS2_PLACEMENT_3D('',#8573,#5967,#5968);
#5072=AXIS2_PLACEMENT_3D('',#8575,#5969,#5970);
#5073=AXIS2_PLACEMENT_3D('',#8576,#5971,#5972);
#5074=AXIS2_PLACEMENT_3D('',#8578,#5973,#5974);
#5075=AXIS2_PLACEMENT_3D('',#8580,#5976,#5977);
#5076=AXIS2_PLACEMENT_3D('',#8582,#5978,#5979);
#5077=AXIS2_PLACEMENT_3D('',#8584,#5981,#5982);
#5078=AXIS2_PLACEMENT_3D('',#8586,#5983,#5984);
#5079=AXIS2_PLACEMENT_3D('',#8588,#5986,#5987);
#5080=AXIS2_PLACEMENT_3D('',#8590,#5988,#5989);
#5081=AXIS2_PLACEMENT_3D('',#8591,#5990,#5991);
#5082=AXIS2_PLACEMENT_3D('',#8593,#5992,#5993);
#5083=AXIS2_PLACEMENT_3D('',#8595,#5995,#5996);
#5084=AXIS2_PLACEMENT_3D('',#8597,#5998,#5999);
#5085=AXIS2_PLACEMENT_3D('',#8598,#6000,#6001);
#5086=AXIS2_PLACEMENT_3D('',#8599,#6002,#6003);
#5087=AXIS2_PLACEMENT_3D('',#8602,#6004,#6005);
#5088=AXIS2_PLACEMENT_3D('',#8603,#6006,#6007);
#5089=AXIS2_PLACEMENT_3D('',#8605,#6008,#6009);
#5090=AXIS2_PLACEMENT_3D('',#8607,#6010,#6011);
#5091=AXIS2_PLACEMENT_3D('',#8608,#6012,#6013);
#5092=AXIS2_PLACEMENT_3D('',#8609,#6014,#6015);
#5093=AXIS2_PLACEMENT_3D('',#8612,#6017,#6018);
#5094=AXIS2_PLACEMENT_3D('',#8613,#6019,#6020);
#5095=AXIS2_PLACEMENT_3D('',#8615,#6021,#6022);
#5096=AXIS2_PLACEMENT_3D('',#8618,#6024,#6025);
#5097=AXIS2_PLACEMENT_3D('',#8619,#6026,#6027);
#5098=AXIS2_PLACEMENT_3D('',#8622,#6029,#6030);
#5099=AXIS2_PLACEMENT_3D('',#8623,#6031,#6032);
#5100=AXIS2_PLACEMENT_3D('',#8624,#6033,#6034);
#5101=AXIS2_PLACEMENT_3D('',#8626,#6035,#6036);
#5102=AXIS2_PLACEMENT_3D('',#8628,#6038,#6039);
#5103=AXIS2_PLACEMENT_3D('',#8630,#6040,#6041);
#5104=AXIS2_PLACEMENT_3D('',#8631,#6042,#6043);
#5105=AXIS2_PLACEMENT_3D('',#8633,#6045,#6046);
#5106=AXIS2_PLACEMENT_3D('',#8634,#6047,#6048);
#5107=AXIS2_PLACEMENT_3D('',#8637,#6049,#6050);
#5108=AXIS2_PLACEMENT_3D('',#8638,#6051,#6052);
#5109=AXIS2_PLACEMENT_3D('',#8640,#6053,#6054);
#5110=AXIS2_PLACEMENT_3D('',#8642,#6055,#6056);
#5111=AXIS2_PLACEMENT_3D('',#8643,#6057,#6058);
#5112=AXIS2_PLACEMENT_3D('',#8644,#6059,#6060);
#5113=AXIS2_PLACEMENT_3D('',#8646,#6061,#6062);
#5114=AXIS2_PLACEMENT_3D('',#8648,#6064,#6065);
#5115=AXIS2_PLACEMENT_3D('',#8650,#6066,#6067);
#5116=AXIS2_PLACEMENT_3D('',#8652,#6068,#6069);
#5117=AXIS2_PLACEMENT_3D('',#8653,#6070,#6071);
#5118=AXIS2_PLACEMENT_3D('',#8655,#6072,#6073);
#5119=AXIS2_PLACEMENT_3D('',#8657,#6075,#6076);
#5120=AXIS2_PLACEMENT_3D('',#8659,#6077,#6078);
#5121=AXIS2_PLACEMENT_3D('',#8661,#6080,#6081);
#5122=AXIS2_PLACEMENT_3D('',#8663,#6082,#6083);
#5123=AXIS2_PLACEMENT_3D('',#8665,#6085,#6086);
#5124=AXIS2_PLACEMENT_3D('',#8666,#6087,#6088);
#5125=AXIS2_PLACEMENT_3D('',#8668,#6090,#6091);
#5126=AXIS2_PLACEMENT_3D('',#8669,#6092,#6093);
#5127=AXIS2_PLACEMENT_3D('',#8672,#6094,#6095);
#5128=AXIS2_PLACEMENT_3D('',#8673,#6096,#6097);
#5129=AXIS2_PLACEMENT_3D('',#8676,#6098,#6099);
#5130=AXIS2_PLACEMENT_3D('',#8677,#6100,#6101);
#5131=AXIS2_PLACEMENT_3D('',#8680,#6102,#6103);
#5132=AXIS2_PLACEMENT_3D('',#8681,#6104,#6105);
#5133=AXIS2_PLACEMENT_3D('',#8684,#6106,#6107);
#5134=AXIS2_PLACEMENT_3D('',#8685,#6108,#6109);
#5135=AXIS2_PLACEMENT_3D('',#8688,#6110,#6111);
#5136=AXIS2_PLACEMENT_3D('',#8689,#6112,#6113);
#5137=AXIS2_PLACEMENT_3D('',#8692,#6114,#6115);
#5138=AXIS2_PLACEMENT_3D('',#8693,#6116,#6117);
#5139=AXIS2_PLACEMENT_3D('',#8696,#6118,#6119);
#5140=AXIS2_PLACEMENT_3D('',#8697,#6120,#6121);
#5141=AXIS2_PLACEMENT_3D('',#8700,#6122,#6123);
#5142=AXIS2_PLACEMENT_3D('',#8701,#6124,#6125);
#5143=AXIS2_PLACEMENT_3D('',#8704,#6126,#6127);
#5144=AXIS2_PLACEMENT_3D('',#8705,#6128,#6129);
#5145=AXIS2_PLACEMENT_3D('',#8706,#6130,#6131);
#5146=AXIS2_PLACEMENT_3D('',#8732,#6132,#6133);
#5147=AXIS2_PLACEMENT_3D('',#8756,#6134,#6135);
#5148=AXIS2_PLACEMENT_3D('',#8757,#6136,#6137);
#5149=AXIS2_PLACEMENT_3D('',#8759,#6138,#6139);
#5150=AXIS2_PLACEMENT_3D('',#8784,#6140,#6141);
#5151=AXIS2_PLACEMENT_3D('',#8809,#6142,#6143);
#5152=AXIS2_PLACEMENT_3D('',#8834,#6144,#6145);
#5153=AXIS2_PLACEMENT_3D('',#8837,#6147,#6148);
#5154=AXIS2_PLACEMENT_3D('',#8839,#6149,#6150);
#5155=AXIS2_PLACEMENT_3D('',#8864,#6151,#6152);
#5156=AXIS2_PLACEMENT_3D('',#8889,#6153,#6154);
#5157=AXIS2_PLACEMENT_3D('',#8914,#6155,#6156);
#5158=AXIS2_PLACEMENT_3D('',#8939,#6157,#6158);
#5159=AXIS2_PLACEMENT_3D('',#8963,#6159,#6160);
#5160=AXIS2_PLACEMENT_3D('',#8964,#6161,#6162);
#5161=AXIS2_PLACEMENT_3D('',#8966,#6163,#6164);
#5162=AXIS2_PLACEMENT_3D('',#8967,#6165,#6166);
#5163=AXIS2_PLACEMENT_3D('',#8968,#6167,#6168);
#5164=AXIS2_PLACEMENT_3D('',#8992,#6169,#6170);
#5165=AXIS2_PLACEMENT_3D('',#8993,#6171,#6172);
#5166=AXIS2_PLACEMENT_3D('',#8995,#6173,#6174);
#5167=AXIS2_PLACEMENT_3D('',#8996,#6175,#6176);
#5168=AXIS2_PLACEMENT_3D('',#8997,#6177,#6178);
#5169=AXIS2_PLACEMENT_3D('',#9021,#6179,#6180);
#5170=AXIS2_PLACEMENT_3D('',#9022,#6181,#6182);
#5171=AXIS2_PLACEMENT_3D('',#9024,#6183,#6184);
#5172=AXIS2_PLACEMENT_3D('',#9025,#6185,#6186);
#5173=AXIS2_PLACEMENT_3D('',#9026,#6187,#6188);
#5174=AXIS2_PLACEMENT_3D('',#9050,#6189,#6190);
#5175=AXIS2_PLACEMENT_3D('',#9051,#6191,#6192);
#5176=AXIS2_PLACEMENT_3D('',#9053,#6193,#6194);
#5177=AXIS2_PLACEMENT_3D('',#9055,#6195,#6196);
#5178=AXIS2_PLACEMENT_3D('',#9056,#6197,#6198);
#5179=AXIS2_PLACEMENT_3D('',#9057,#6199,#6200);
#5180=AXIS2_PLACEMENT_3D('',#9081,#6201,#6202);
#5181=AXIS2_PLACEMENT_3D('',#9082,#6203,#6204);
#5182=AXIS2_PLACEMENT_3D('',#9084,#6205,#6206);
#5183=AXIS2_PLACEMENT_3D('',#9085,#6207,#6208);
#5184=AXIS2_PLACEMENT_3D('',#9086,#6209,#6210);
#5185=AXIS2_PLACEMENT_3D('',#9110,#6211,#6212);
#5186=AXIS2_PLACEMENT_3D('',#9111,#6213,#6214);
#5187=AXIS2_PLACEMENT_3D('',#9113,#6215,#6216);
#5188=AXIS2_PLACEMENT_3D('',#9114,#6217,#6218);
#5189=AXIS2_PLACEMENT_3D('',#9115,#6219,#6220);
#5190=AXIS2_PLACEMENT_3D('',#9139,#6221,#6222);
#5191=AXIS2_PLACEMENT_3D('',#9140,#6223,#6224);
#5192=AXIS2_PLACEMENT_3D('',#9142,#6225,#6226);
#5193=AXIS2_PLACEMENT_3D('',#9143,#6227,#6228);
#5194=AXIS2_PLACEMENT_3D('',#9144,#6229,#6230);
#5195=AXIS2_PLACEMENT_3D('',#9168,#6231,#6232);
#5196=AXIS2_PLACEMENT_3D('',#9169,#6233,#6234);
#5197=AXIS2_PLACEMENT_3D('',#9171,#6235,#6236);
#5198=AXIS2_PLACEMENT_3D('',#9174,#6238,#6239);
#5199=AXIS2_PLACEMENT_3D('',#9198,#6240,#6241);
#5200=AXIS2_PLACEMENT_3D('',#9199,#6242,#6243);
#5201=AXIS2_PLACEMENT_3D('',#9200,#6244,#6245);
#5202=AXIS2_PLACEMENT_3D('',#9201,#6246,#6247);
#5203=AXIS2_PLACEMENT_3D('',#9202,#6248,#6249);
#5204=AXIS2_PLACEMENT_3D('',#9203,#6250,#6251);
#5205=AXIS2_PLACEMENT_3D('',#9204,#6252,#6253);
#5206=AXIS2_PLACEMENT_3D('',#9205,#6254,#6255);
#5207=AXIS2_PLACEMENT_3D('',#9206,#6256,#6257);
#5208=AXIS2_PLACEMENT_3D('',#9208,#6258,#6259);
#5209=AXIS2_PLACEMENT_3D('',#9210,#6260,#6261);
#5210=AXIS2_PLACEMENT_3D('',#9211,#6262,#6263);
#5211=AXIS2_PLACEMENT_3D('',#9213,#6264,#6265);
#5212=AXIS2_PLACEMENT_3D('',#9215,#6267,#6268);
#5213=AXIS2_PLACEMENT_3D('',#9217,#6269,#6270);
#5214=AXIS2_PLACEMENT_3D('',#9218,#6271,#6272);
#5215=AXIS2_PLACEMENT_3D('',#9220,#6274,#6275);
#5216=AXIS2_PLACEMENT_3D('',#9222,#6276,#6277);
#5217=AXIS2_PLACEMENT_3D('',#9224,#6278,#6279);
#5218=AXIS2_PLACEMENT_3D('',#9225,#6280,#6281);
#5219=AXIS2_PLACEMENT_3D('',#9227,#6282,#6283);
#5220=AXIS2_PLACEMENT_3D('',#9229,#6285,#6286);
#5221=AXIS2_PLACEMENT_3D('',#9231,#6287,#6288);
#5222=AXIS2_PLACEMENT_3D('',#9232,#6289,#6290);
#5223=AXIS2_PLACEMENT_3D('',#9234,#6292,#6293);
#5224=AXIS2_PLACEMENT_3D('',#9235,#6294,#6295);
#5225=AXIS2_PLACEMENT_3D('',#9236,#6296,#6297);
#5226=AXIS2_PLACEMENT_3D('',#9237,#6298,#6299);
#5227=AXIS2_PLACEMENT_3D('',#9238,#6300,#6301);
#5228=AXIS2_PLACEMENT_3D('',#9239,#6302,#6303);
#5229=AXIS2_PLACEMENT_3D('',#9240,#6304,#6305);
#5230=AXIS2_PLACEMENT_3D('',#9242,#6306,#6307);
#5231=AXIS2_PLACEMENT_3D('',#9243,#6308,#6309);
#5232=AXIS2_PLACEMENT_3D('',#9252,#6314,#6315);
#5233=AXIS2_PLACEMENT_3D('',#9258,#6319,#6320);
#5234=AXIS2_PLACEMENT_3D('',#9264,#6324,#6325);
#5235=AXIS2_PLACEMENT_3D('',#9270,#6329,#6330);
#5236=AXIS2_PLACEMENT_3D('',#9276,#6334,#6335);
#5237=AXIS2_PLACEMENT_3D('',#9279,#6338,#6339);
#5238=AXIS2_PLACEMENT_3D('',#9280,#6340,#6341);
#5239=AXIS2_PLACEMENT_3D('',#9282,#6342,#6343);
#5240=AXIS2_PLACEMENT_3D('',#9283,#6344,#6345);
#5241=AXIS2_PLACEMENT_3D('',#9285,#6346,#6347);
#5242=AXIS2_PLACEMENT_3D('',#9287,#6349,#6350);
#5243=AXIS2_PLACEMENT_3D('',#9289,#6352,#6353);
#5244=AXIS2_PLACEMENT_3D('',#9290,#6354,#6355);
#5245=AXIS2_PLACEMENT_3D('',#9291,#6356,#6357);
#5246=AXIS2_PLACEMENT_3D('',#9293,#6358,#6359);
#5247=AXIS2_PLACEMENT_3D('',#9296,#6361,#6362);
#5248=AXIS2_PLACEMENT_3D('',#9297,#6363,#6364);
#5249=AXIS2_PLACEMENT_3D('',#9298,#6365,#6366);
#5250=AXIS2_PLACEMENT_3D('',#9300,#6367,#6368);
#5251=AXIS2_PLACEMENT_3D('',#9303,#6370,#6371);
#5252=AXIS2_PLACEMENT_3D('',#9304,#6372,#6373);
#5253=AXIS2_PLACEMENT_3D('',#9305,#6374,#6375);
#5254=AXIS2_PLACEMENT_3D('',#9307,#6376,#6377);
#5255=AXIS2_PLACEMENT_3D('',#9310,#6379,#6380);
#5256=AXIS2_PLACEMENT_3D('',#9311,#6381,#6382);
#5257=AXIS2_PLACEMENT_3D('',#9312,#6383,#6384);
#5258=AXIS2_PLACEMENT_3D('',#9314,#6385,#6386);
#5259=AXIS2_PLACEMENT_3D('',#9317,#6388,#6389);
#5260=AXIS2_PLACEMENT_3D('',#9318,#6390,#6391);
#5261=AXIS2_PLACEMENT_3D('',#9319,#6392,#6393);
#5262=AXIS2_PLACEMENT_3D('',#9321,#6394,#6395);
#5263=AXIS2_PLACEMENT_3D('',#9324,#6397,#6398);
#5264=AXIS2_PLACEMENT_3D('',#9325,#6399,#6400);
#5265=AXIS2_PLACEMENT_3D('',#9326,#6401,#6402);
#5266=AXIS2_PLACEMENT_3D('',#9328,#6403,#6404);
#5267=AXIS2_PLACEMENT_3D('',#9331,#6406,#6407);
#5268=AXIS2_PLACEMENT_3D('',#9332,#6408,#6409);
#5269=AXIS2_PLACEMENT_3D('',#9333,#6410,#6411);
#5270=AXIS2_PLACEMENT_3D('',#9335,#6412,#6413);
#5271=AXIS2_PLACEMENT_3D('',#9338,#6415,#6416);
#5272=AXIS2_PLACEMENT_3D('',#9339,#6417,#6418);
#5273=AXIS2_PLACEMENT_3D('',#9340,#6419,#6420);
#5274=AXIS2_PLACEMENT_3D('',#9342,#6421,#6422);
#5275=AXIS2_PLACEMENT_3D('',#9345,#6424,#6425);
#5276=AXIS2_PLACEMENT_3D('',#9346,#6426,#6427);
#5277=AXIS2_PLACEMENT_3D('',#9347,#6428,#6429);
#5278=AXIS2_PLACEMENT_3D('',#9349,#6430,#6431);
#5279=AXIS2_PLACEMENT_3D('',#9352,#6433,#6434);
#5280=AXIS2_PLACEMENT_3D('',#9353,#6435,#6436);
#5281=AXIS2_PLACEMENT_3D('',#9354,#6437,#6438);
#5282=AXIS2_PLACEMENT_3D('',#9356,#6439,#6440);
#5283=AXIS2_PLACEMENT_3D('',#9359,#6442,#6443);
#5284=AXIS2_PLACEMENT_3D('',#9360,#6444,#6445);
#5285=AXIS2_PLACEMENT_3D('',#9361,#6446,#6447);
#5286=AXIS2_PLACEMENT_3D('',#9363,#6448,#6449);
#5287=AXIS2_PLACEMENT_3D('',#9366,#6451,#6452);
#5288=AXIS2_PLACEMENT_3D('',#9367,#6453,#6454);
#5289=AXIS2_PLACEMENT_3D('',#9368,#6455,#6456);
#5290=AXIS2_PLACEMENT_3D('',#9370,#6457,#6458);
#5291=AXIS2_PLACEMENT_3D('',#9373,#6460,#6461);
#5292=AXIS2_PLACEMENT_3D('',#9374,#6462,#6463);
#5293=AXIS2_PLACEMENT_3D('',#9375,#6464,#6465);
#5294=AXIS2_PLACEMENT_3D('',#9377,#6466,#6467);
#5295=AXIS2_PLACEMENT_3D('',#9380,#6469,#6470);
#5296=AXIS2_PLACEMENT_3D('',#9381,#6471,#6472);
#5297=AXIS2_PLACEMENT_3D('',#9382,#6473,#6474);
#5298=AXIS2_PLACEMENT_3D('',#9384,#6475,#6476);
#5299=AXIS2_PLACEMENT_3D('',#9387,#6478,#6479);
#5300=AXIS2_PLACEMENT_3D('',#9388,#6480,#6481);
#5301=AXIS2_PLACEMENT_3D('',#9389,#6482,#6483);
#5302=AXIS2_PLACEMENT_3D('',#9391,#6484,#6485);
#5303=AXIS2_PLACEMENT_3D('',#9394,#6487,#6488);
#5304=AXIS2_PLACEMENT_3D('',#9395,#6489,#6490);
#5305=AXIS2_PLACEMENT_3D('',#9396,#6491,#6492);
#5306=AXIS2_PLACEMENT_3D('',#9398,#6493,#6494);
#5307=AXIS2_PLACEMENT_3D('',#9401,#6496,#6497);
#5308=AXIS2_PLACEMENT_3D('',#9402,#6498,#6499);
#5309=AXIS2_PLACEMENT_3D('',#9403,#6500,#6501);
#5310=AXIS2_PLACEMENT_3D('',#9405,#6502,#6503);
#5311=AXIS2_PLACEMENT_3D('',#9408,#6505,#6506);
#5312=AXIS2_PLACEMENT_3D('',#9409,#6507,#6508);
#5313=AXIS2_PLACEMENT_3D('',#9410,#6509,#6510);
#5314=AXIS2_PLACEMENT_3D('',#9412,#6511,#6512);
#5315=AXIS2_PLACEMENT_3D('',#9415,#6514,#6515);
#5316=AXIS2_PLACEMENT_3D('',#9416,#6516,#6517);
#5317=AXIS2_PLACEMENT_3D('',#9417,#6518,#6519);
#5318=AXIS2_PLACEMENT_3D('',#9419,#6520,#6521);
#5319=AXIS2_PLACEMENT_3D('',#9422,#6523,#6524);
#5320=AXIS2_PLACEMENT_3D('',#9423,#6525,#6526);
#5321=AXIS2_PLACEMENT_3D('',#9424,#6527,#6528);
#5322=AXIS2_PLACEMENT_3D('',#9426,#6529,#6530);
#5323=AXIS2_PLACEMENT_3D('',#9429,#6532,#6533);
#5324=AXIS2_PLACEMENT_3D('',#9430,#6534,#6535);
#5325=AXIS2_PLACEMENT_3D('',#9431,#6536,#6537);
#5326=AXIS2_PLACEMENT_3D('',#9433,#6538,#6539);
#5327=AXIS2_PLACEMENT_3D('',#9436,#6541,#6542);
#5328=AXIS2_PLACEMENT_3D('',#9437,#6543,#6544);
#5329=AXIS2_PLACEMENT_3D('',#9439,#6545,#6546);
#5330=AXIS2_PLACEMENT_3D('',#9442,#6548,#6549);
#5331=AXIS2_PLACEMENT_3D('',#9443,#6550,#6551);
#5332=AXIS2_PLACEMENT_3D('',#9445,#6552,#6553);
#5333=AXIS2_PLACEMENT_3D('',#9448,#6555,#6556);
#5334=AXIS2_PLACEMENT_3D('',#9449,#6557,#6558);
#5335=AXIS2_PLACEMENT_3D('',#9451,#6559,#6560);
#5336=AXIS2_PLACEMENT_3D('',#9454,#6562,#6563);
#5337=AXIS2_PLACEMENT_3D('',#9455,#6564,#6565);
#5338=AXIS2_PLACEMENT_3D('',#9457,#6566,#6567);
#5339=AXIS2_PLACEMENT_3D('',#9460,#6569,#6570);
#5340=AXIS2_PLACEMENT_3D('',#9461,#6571,#6572);
#5341=AXIS2_PLACEMENT_3D('',#9463,#6573,#6574);
#5342=AXIS2_PLACEMENT_3D('',#9466,#6576,#6577);
#5343=AXIS2_PLACEMENT_3D('',#9467,#6578,#6579);
#5344=AXIS2_PLACEMENT_3D('',#9469,#6580,#6581);
#5345=AXIS2_PLACEMENT_3D('',#9472,#6583,#6584);
#5346=AXIS2_PLACEMENT_3D('',#9473,#6585,#6586);
#5347=AXIS2_PLACEMENT_3D('',#9475,#6587,#6588);
#5348=AXIS2_PLACEMENT_3D('',#9478,#6590,#6591);
#5349=AXIS2_PLACEMENT_3D('',#9479,#6592,#6593);
#5350=AXIS2_PLACEMENT_3D('',#9481,#6594,#6595);
#5351=AXIS2_PLACEMENT_3D('',#9483,#6596,#6597);
#5352=AXIS2_PLACEMENT_3D('',#9484,#6598,#6599);
#5353=AXIS2_PLACEMENT_3D('',#9487,#6601,#6602);
#5354=AXIS2_PLACEMENT_3D('',#9488,#6603,#6604);
#5355=AXIS2_PLACEMENT_3D('',#9490,#6605,#6606);
#5356=AXIS2_PLACEMENT_3D('',#9491,#6607,#6608);
#5357=AXIS2_PLACEMENT_3D('',#9493,#6609,#6610);
#5358=AXIS2_PLACEMENT_3D('',#9495,#6611,#6612);
#5359=AXIS2_PLACEMENT_3D('',#9496,#6613,#6614);
#5360=AXIS2_PLACEMENT_3D('',#9498,#6615,#6616);
#5361=AXIS2_PLACEMENT_3D('',#9500,#6618,#6619);
#5362=AXIS2_PLACEMENT_3D('',#9502,#6620,#6621);
#5363=AXIS2_PLACEMENT_3D('',#9504,#6623,#6624);
#5364=AXIS2_PLACEMENT_3D('',#9505,#6625,#6626);
#5365=AXIS2_PLACEMENT_3D('',#9508,#6628,#6629);
#5366=AXIS2_PLACEMENT_3D('',#9509,#6630,#6631);
#5367=AXIS2_PLACEMENT_3D('',#9512,#6633,#6634);
#5368=AXIS2_PLACEMENT_3D('',#9513,#6635,#6636);
#5369=AXIS2_PLACEMENT_3D('',#9514,#6637,#6638);
#5370=AXIS2_PLACEMENT_3D('',#9515,#6639,#6640);
#5371=AXIS2_PLACEMENT_3D('',#9517,#6641,#6642);
#5372=AXIS2_PLACEMENT_3D('',#9520,#6644,#6645);
#5373=AXIS2_PLACEMENT_3D('',#9521,#6646,#6647);
#5374=AXIS2_PLACEMENT_3D('',#9523,#6648,#6649);
#5375=AXIS2_PLACEMENT_3D('',#9526,#6651,#6652);
#5376=AXIS2_PLACEMENT_3D('',#9527,#6653,#6654);
#5377=AXIS2_PLACEMENT_3D('',#9528,#6655,#6656);
#5378=AXIS2_PLACEMENT_3D('',#9529,#6657,#6658);
#5379=AXIS2_PLACEMENT_3D('',#9530,#6659,#6660);
#5380=AXIS2_PLACEMENT_3D('',#9532,#6661,#6662);
#5381=AXIS2_PLACEMENT_3D('',#9535,#6664,#6665);
#5382=AXIS2_PLACEMENT_3D('',#9536,#6666,#6667);
#5383=AXIS2_PLACEMENT_3D('',#9538,#6668,#6669);
#5384=AXIS2_PLACEMENT_3D('',#9541,#6671,#6672);
#5385=AXIS2_PLACEMENT_3D('',#9542,#6673,#6674);
#5386=AXIS2_PLACEMENT_3D('',#9544,#6675,#6676);
#5387=AXIS2_PLACEMENT_3D('',#9547,#6678,#6679);
#5388=AXIS2_PLACEMENT_3D('',#9548,#6680,#6681);
#5389=AXIS2_PLACEMENT_3D('',#9550,#6682,#6683);
#5390=AXIS2_PLACEMENT_3D('',#9553,#6685,#6686);
#5391=AXIS2_PLACEMENT_3D('',#9554,#6687,#6688);
#5392=AXIS2_PLACEMENT_3D('',#9556,#6689,#6690);
#5393=AXIS2_PLACEMENT_3D('',#9559,#6692,#6693);
#5394=AXIS2_PLACEMENT_3D('',#9560,#6694,#6695);
#5395=AXIS2_PLACEMENT_3D('',#9562,#6696,#6697);
#5396=AXIS2_PLACEMENT_3D('',#9563,#6698,#6699);
#5397=AXIS2_PLACEMENT_3D('',#9566,#6701,#6702);
#5398=AXIS2_PLACEMENT_3D('',#9567,#6703,#6704);
#5399=AXIS2_PLACEMENT_3D('',#9569,#6705,#6706);
#5400=AXIS2_PLACEMENT_3D('',#9572,#6708,#6709);
#5401=AXIS2_PLACEMENT_3D('',#9573,#6710,#6711);
#5402=AXIS2_PLACEMENT_3D('',#9574,#6712,#6713);
#5403=AXIS2_PLACEMENT_3D('',#9575,#6714,#6715);
#5404=AXIS2_PLACEMENT_3D('',#9576,#6716,#6717);
#5405=AXIS2_PLACEMENT_3D('',#9578,#6718,#6719);
#5406=AXIS2_PLACEMENT_3D('',#9581,#6721,#6722);
#5407=AXIS2_PLACEMENT_3D('',#9582,#6723,#6724);
#5408=AXIS2_PLACEMENT_3D('',#9584,#6725,#6726);
#5409=AXIS2_PLACEMENT_3D('',#9587,#6728,#6729);
#5410=AXIS2_PLACEMENT_3D('',#9588,#6730,#6731);
#5411=AXIS2_PLACEMENT_3D('',#9590,#6732,#6733);
#5412=AXIS2_PLACEMENT_3D('',#9593,#6735,#6736);
#5413=AXIS2_PLACEMENT_3D('',#9594,#6737,#6738);
#5414=AXIS2_PLACEMENT_3D('',#9596,#6739,#6740);
#5415=AXIS2_PLACEMENT_3D('',#9599,#6742,#6743);
#5416=AXIS2_PLACEMENT_3D('',#9600,#6744,#6745);
#5417=AXIS2_PLACEMENT_3D('',#9602,#6746,#6747);
#5418=AXIS2_PLACEMENT_3D('',#9605,#6749,#6750);
#5419=AXIS2_PLACEMENT_3D('',#9606,#6751,#6752);
#5420=AXIS2_PLACEMENT_3D('',#9608,#6753,#6754);
#5421=AXIS2_PLACEMENT_3D('',#9611,#6756,#6757);
#5422=AXIS2_PLACEMENT_3D('',#9612,#6758,#6759);
#5423=AXIS2_PLACEMENT_3D('',#9614,#6760,#6761);
#5424=AXIS2_PLACEMENT_3D('',#9617,#6763,#6764);
#5425=AXIS2_PLACEMENT_3D('',#9618,#6765,#6766);
#5426=AXIS2_PLACEMENT_3D('',#9620,#6767,#6768);
#5427=AXIS2_PLACEMENT_3D('',#9623,#6770,#6771);
#5428=AXIS2_PLACEMENT_3D('',#9624,#6772,#6773);
#5429=AXIS2_PLACEMENT_3D('',#9626,#6774,#6775);
#5430=AXIS2_PLACEMENT_3D('',#9629,#6777,#6778);
#5431=AXIS2_PLACEMENT_3D('',#9630,#6779,#6780);
#5432=AXIS2_PLACEMENT_3D('',#9632,#6781,#6782);
#5433=AXIS2_PLACEMENT_3D('',#9635,#6784,#6785);
#5434=AXIS2_PLACEMENT_3D('',#9636,#6786,#6787);
#5435=AXIS2_PLACEMENT_3D('',#9638,#6788,#6789);
#5436=AXIS2_PLACEMENT_3D('',#9641,#6791,#6792);
#5437=AXIS2_PLACEMENT_3D('',#9642,#6793,#6794);
#5438=AXIS2_PLACEMENT_3D('',#9644,#6795,#6796);
#5439=AXIS2_PLACEMENT_3D('',#9647,#6798,#6799);
#5440=AXIS2_PLACEMENT_3D('',#9648,#6800,#6801);
#5441=AXIS2_PLACEMENT_3D('',#9650,#6802,#6803);
#5442=AXIS2_PLACEMENT_3D('',#9653,#6805,#6806);
#5443=AXIS2_PLACEMENT_3D('',#9654,#6807,#6808);
#5444=AXIS2_PLACEMENT_3D('',#9656,#6809,#6810);
#5445=AXIS2_PLACEMENT_3D('',#9659,#6812,#6813);
#5446=AXIS2_PLACEMENT_3D('',#9660,#6814,#6815);
#5447=AXIS2_PLACEMENT_3D('',#9662,#6816,#6817);
#5448=AXIS2_PLACEMENT_3D('',#9665,#6819,#6820);
#5449=AXIS2_PLACEMENT_3D('',#9666,#6821,#6822);
#5450=AXIS2_PLACEMENT_3D('',#9668,#6823,#6824);
#5451=AXIS2_PLACEMENT_3D('',#9671,#6826,#6827);
#5452=AXIS2_PLACEMENT_3D('',#9672,#6828,#6829);
#5453=AXIS2_PLACEMENT_3D('',#9674,#6830,#6831);
#5454=AXIS2_PLACEMENT_3D('',#9677,#6833,#6834);
#5455=AXIS2_PLACEMENT_3D('',#9678,#6835,#6836);
#5456=AXIS2_PLACEMENT_3D('',#9680,#6837,#6838);
#5457=AXIS2_PLACEMENT_3D('',#9683,#6840,#6841);
#5458=AXIS2_PLACEMENT_3D('',#9684,#6842,#6843);
#5459=AXIS2_PLACEMENT_3D('',#9685,#6844,#6845);
#5460=AXIS2_PLACEMENT_3D('',#9686,#6846,#6847);
#5461=AXIS2_PLACEMENT_3D('',#9687,#6848,#6849);
#5462=AXIS2_PLACEMENT_3D('',#9689,#6850,#6851);
#5463=AXIS2_PLACEMENT_3D('',#9690,#6852,#6853);
#5464=AXIS2_PLACEMENT_3D('',#9692,#6854,#6855);
#5465=AXIS2_PLACEMENT_3D('',#9694,#6857,#6858);
#5466=AXIS2_PLACEMENT_3D('',#9696,#6859,#6860);
#5467=AXIS2_PLACEMENT_3D('',#9698,#6862,#6863);
#5468=AXIS2_PLACEMENT_3D('',#9700,#6864,#6865);
#5469=AXIS2_PLACEMENT_3D('',#9702,#6867,#6868);
#5470=AXIS2_PLACEMENT_3D('',#9704,#6869,#6870);
#5471=AXIS2_PLACEMENT_3D('',#9705,#6871,#6872);
#5472=AXIS2_PLACEMENT_3D('',#9707,#6873,#6874);
#5473=AXIS2_PLACEMENT_3D('',#9709,#6876,#6877);
#5474=AXIS2_PLACEMENT_3D('',#9711,#6878,#6879);
#5475=AXIS2_PLACEMENT_3D('',#9713,#6881,#6882);
#5476=AXIS2_PLACEMENT_3D('',#9715,#6883,#6884);
#5477=AXIS2_PLACEMENT_3D('',#9717,#6886,#6887);
#5478=AXIS2_PLACEMENT_3D('',#9718,#6888,#6889);
#5479=AXIS2_PLACEMENT_3D('',#9727,#6894,#6895);
#5480=AXIS2_PLACEMENT_3D('',#9733,#6899,#6900);
#5481=AXIS2_PLACEMENT_3D('',#9739,#6904,#6905);
#5482=AXIS2_PLACEMENT_3D('',#9745,#6909,#6910);
#5483=AXIS2_PLACEMENT_3D('',#9751,#6914,#6915);
#5484=AXIS2_PLACEMENT_3D('',#9754,#6918,#6919);
#5485=AXIS2_PLACEMENT_3D('',#9755,#6920,#6921);
#5486=AXIS2_PLACEMENT_3D('',#9756,#6922,#6923);
#5487=AXIS2_PLACEMENT_3D('',#9757,#6924,#6925);
#5488=AXIS2_PLACEMENT_3D('',#9758,#6926,#6927);
#5489=AXIS2_PLACEMENT_3D('',#9759,#6928,#6929);
#5490=AXIS2_PLACEMENT_3D('',#9760,#6930,#6931);
#5491=AXIS2_PLACEMENT_3D('',#9761,#6932,#6933);
#5492=AXIS2_PLACEMENT_3D('',#9762,#6934,#6935);
#5493=AXIS2_PLACEMENT_3D('',#9763,#6936,#6937);
#5494=AXIS2_PLACEMENT_3D('',#9764,#6938,#6939);
#5495=AXIS2_PLACEMENT_3D('',#9765,#6940,#6941);
#5496=AXIS2_PLACEMENT_3D('',#9766,#6942,#6943);
#5497=AXIS2_PLACEMENT_3D('',#9767,#6944,#6945);
#5498=AXIS2_PLACEMENT_3D('',#9768,#6946,#6947);
#5499=AXIS2_PLACEMENT_3D('',#9769,#6948,#6949);
#5500=AXIS2_PLACEMENT_3D('',#9770,#6950,#6951);
#5501=AXIS2_PLACEMENT_3D('',#9771,#6952,#6953);
#5502=AXIS2_PLACEMENT_3D('',#9772,#6954,#6955);
#5503=AXIS2_PLACEMENT_3D('',#9773,#6956,#6957);
#5504=AXIS2_PLACEMENT_3D('',#9774,#6958,#6959);
#5505=AXIS2_PLACEMENT_3D('',#9775,#6960,#6961);
#5506=AXIS2_PLACEMENT_3D('',#9776,#6962,#6963);
#5507=AXIS2_PLACEMENT_3D('',#9777,#6964,#6965);
#5508=AXIS2_PLACEMENT_3D('',#9778,#6966,#6967);
#5509=AXIS2_PLACEMENT_3D('',#9779,#6968,#6969);
#5510=AXIS2_PLACEMENT_3D('',#9780,#6970,#6971);
#5511=AXIS2_PLACEMENT_3D('',#9781,#6972,#6973);
#5512=AXIS2_PLACEMENT_3D('',#9782,#6974,#6975);
#5513=AXIS2_PLACEMENT_3D('',#9783,#6976,#6977);
#5514=AXIS2_PLACEMENT_3D('',#9784,#6978,#6979);
#5515=AXIS2_PLACEMENT_3D('',#9785,#6980,#6981);
#5516=AXIS2_PLACEMENT_3D('',#9786,#6982,#6983);
#5517=AXIS2_PLACEMENT_3D('',#9787,#6984,#6985);
#5518=AXIS2_PLACEMENT_3D('',#9788,#6986,#6987);
#5519=AXIS2_PLACEMENT_3D('',#9789,#6988,#6989);
#5520=AXIS2_PLACEMENT_3D('',#9790,#6990,#6991);
#5521=AXIS2_PLACEMENT_3D('',#9791,#6992,#6993);
#5522=AXIS2_PLACEMENT_3D('',#9792,#6994,#6995);
#5523=AXIS2_PLACEMENT_3D('',#9793,#6996,#6997);
#5524=AXIS2_PLACEMENT_3D('',#9795,#6998,#6999);
#5525=AXIS2_PLACEMENT_3D('',#9796,#7000,#7001);
#5526=AXIS2_PLACEMENT_3D('',#9798,#7002,#7003);
#5527=AXIS2_PLACEMENT_3D('',#9800,#7004,#7005);
#5528=AXIS2_PLACEMENT_3D('',#9801,#7006,#7007);
#5529=AXIS2_PLACEMENT_3D('',#9803,#7008,#7009);
#5530=AXIS2_PLACEMENT_3D('',#9805,#7010,#7011);
#5531=AXIS2_PLACEMENT_3D('',#9806,#7012,#7013);
#5532=AXIS2_PLACEMENT_3D('',#9808,#7015,#7016);
#5533=AXIS2_PLACEMENT_3D('',#9810,#7018,#7019);
#5534=AXIS2_PLACEMENT_3D('',#9812,#7020,#7021);
#5535=AXIS2_PLACEMENT_3D('',#9814,#7023,#7024);
#5536=AXIS2_PLACEMENT_3D('',#9815,#7025,#7026);
#5537=AXIS2_PLACEMENT_3D('',#9816,#7027,#7028);
#5538=AXIS2_PLACEMENT_3D('',#9820,#7030,#7031);
#5539=AXIS2_PLACEMENT_3D('',#9821,#7032,#7033);
#5540=AXIS2_PLACEMENT_3D('',#9830,#7034,#7035);
#5541=AXIS2_PLACEMENT_3D('',#9879,#7037,#7038);
#5542=AXIS2_PLACEMENT_3D('',#9881,#7040,#7041);
#5543=AXIS2_PLACEMENT_3D('',#9883,#7042,#7043);
#5544=AXIS2_PLACEMENT_3D('',#9886,#7045,#7046);
#5545=AXIS2_PLACEMENT_3D('',#9887,#7047,#7048);
#5546=AXIS2_PLACEMENT_3D('',#9889,#7049,#7050);
#5547=AXIS2_PLACEMENT_3D('',#9892,#7052,#7053);
#5548=AXIS2_PLACEMENT_3D('',#9893,#7054,#7055);
#5549=AXIS2_PLACEMENT_3D('',#9894,#7056,#7057);
#5550=AXIS2_PLACEMENT_3D('',#9895,#7058,#7059);
#5551=AXIS2_PLACEMENT_3D('',#9896,#7060,#7061);
#5552=AXIS2_PLACEMENT_3D('',#9905,#7066,#7067);
#5553=AXIS2_PLACEMENT_3D('',#9911,#7071,#7072);
#5554=AXIS2_PLACEMENT_3D('',#9917,#7076,#7077);
#5555=AXIS2_PLACEMENT_3D('',#9923,#7081,#7082);
#5556=AXIS2_PLACEMENT_3D('',#9929,#7086,#7087);
#5557=AXIS2_PLACEMENT_3D('',#9932,#7090,#7091);
#5558=AXIS2_PLACEMENT_3D('',#9933,#7092,#7093);
#5559=AXIS2_PLACEMENT_3D('',#9935,#7094,#7095);
#5560=AXIS2_PLACEMENT_3D('',#9936,#7096,#7097);
#5561=AXIS2_PLACEMENT_3D('',#9938,#7098,#7099);
#5562=AXIS2_PLACEMENT_3D('',#9940,#7101,#7102);
#5563=AXIS2_PLACEMENT_3D('',#9942,#7103,#7104);
#5564=AXIS2_PLACEMENT_3D('',#9944,#7106,#7107);
#5565=AXIS2_PLACEMENT_3D('',#9946,#7108,#7109);
#5566=AXIS2_PLACEMENT_3D('',#9948,#7111,#7112);
#5567=AXIS2_PLACEMENT_3D('',#9949,#7113,#7114);
#5568=AXIS2_PLACEMENT_3D('',#9950,#7115,#7116);
#5569=AXIS2_PLACEMENT_3D('',#9951,#7117,#7118);
#5570=AXIS2_PLACEMENT_3D('',#9952,#7119,#7120);
#5571=AXIS2_PLACEMENT_3D('',#9953,#7121,#7122);
#5572=AXIS2_PLACEMENT_3D('',#9954,#7123,#7124);
#5573=DIRECTION('axis',(0.,0.,1.));
#5574=DIRECTION('refdir',(1.,0.,0.));
#5575=DIRECTION('axis',(0.,0.,1.));
#5576=DIRECTION('refdir',(1.,0.,0.));
#5577=DIRECTION('axis',(0.,0.,1.));
#5578=DIRECTION('refdir',(1.,0.,0.));
#5579=DIRECTION('center_axis',(0.,0.,1.));
#5580=DIRECTION('ref_axis',(1.,0.,0.));
#5581=DIRECTION('center_axis',(0.,0.,1.));
#5582=DIRECTION('ref_axis',(1.,0.,0.));
#5583=DIRECTION('',(0.,0.,1.));
#5584=DIRECTION('center_axis',(0.,0.,-1.));
#5585=DIRECTION('ref_axis',(1.,0.,0.));
#5586=DIRECTION('center_axis',(0.,0.,1.));
#5587=DIRECTION('ref_axis',(1.,0.,0.));
#5588=DIRECTION('center_axis',(0.,0.,1.));
#5589=DIRECTION('ref_axis',(1.,0.,0.));
#5590=DIRECTION('',(0.,0.,1.));
#5591=DIRECTION('center_axis',(0.,0.,-1.));
#5592=DIRECTION('ref_axis',(1.,0.,0.));
#5593=DIRECTION('center_axis',(0.,0.,1.));
#5594=DIRECTION('ref_axis',(1.,0.,0.));
#5595=DIRECTION('center_axis',(0.,0.,1.));
#5596=DIRECTION('ref_axis',(1.,0.,0.));
#5597=DIRECTION('',(0.,0.,1.));
#5598=DIRECTION('center_axis',(0.,0.,-1.));
#5599=DIRECTION('ref_axis',(1.,0.,0.));
#5600=DIRECTION('center_axis',(0.,0.,1.));
#5601=DIRECTION('ref_axis',(1.,0.,0.));
#5602=DIRECTION('center_axis',(0.,0.,1.));
#5603=DIRECTION('ref_axis',(1.,0.,0.));
#5604=DIRECTION('',(0.,0.,1.));
#5605=DIRECTION('center_axis',(0.,0.,-1.));
#5606=DIRECTION('ref_axis',(1.,0.,0.));
#5607=DIRECTION('center_axis',(0.,0.,1.));
#5608=DIRECTION('ref_axis',(1.,0.,0.));
#5609=DIRECTION('center_axis',(0.,0.,1.));
#5610=DIRECTION('ref_axis',(1.,0.,0.));
#5611=DIRECTION('',(0.,0.,1.));
#5612=DIRECTION('center_axis',(0.,0.,-1.));
#5613=DIRECTION('ref_axis',(1.,0.,0.));
#5614=DIRECTION('center_axis',(0.,0.,1.));
#5615=DIRECTION('ref_axis',(1.,0.,0.));
#5616=DIRECTION('center_axis',(0.,0.,1.));
#5617=DIRECTION('ref_axis',(1.,0.,0.));
#5618=DIRECTION('',(0.,0.,1.));
#5619=DIRECTION('center_axis',(0.,0.,-1.));
#5620=DIRECTION('ref_axis',(1.,0.,0.));
#5621=DIRECTION('center_axis',(0.,0.,1.));
#5622=DIRECTION('ref_axis',(1.,0.,0.));
#5623=DIRECTION('center_axis',(0.,0.,1.));
#5624=DIRECTION('ref_axis',(1.,0.,0.));
#5625=DIRECTION('',(0.,0.,1.));
#5626=DIRECTION('center_axis',(0.,0.,-1.));
#5627=DIRECTION('ref_axis',(1.,0.,0.));
#5628=DIRECTION('center_axis',(0.,1.,0.));
#5629=DIRECTION('ref_axis',(-1.,0.,0.));
#5630=DIRECTION('',(-1.,0.,0.));
#5631=DIRECTION('',(0.,0.,1.));
#5632=DIRECTION('',(-1.,0.,0.));
#5633=DIRECTION('',(0.,0.,1.));
#5634=DIRECTION('center_axis',(1.,0.,0.));
#5635=DIRECTION('ref_axis',(0.,1.,0.));
#5636=DIRECTION('',(0.,1.,0.));
#5637=DIRECTION('',(0.,1.,0.));
#5638=DIRECTION('',(0.,0.,1.));
#5639=DIRECTION('center_axis',(0.,-1.,0.));
#5640=DIRECTION('ref_axis',(1.,0.,0.));
#5641=DIRECTION('',(1.,0.,0.));
#5642=DIRECTION('',(1.,0.,0.));
#5643=DIRECTION('',(0.,0.,1.));
#5644=DIRECTION('center_axis',(-1.,0.,0.));
#5645=DIRECTION('ref_axis',(0.,-1.,0.));
#5646=DIRECTION('',(0.,-1.,0.));
#5647=DIRECTION('',(0.,-1.,0.));
#5648=DIRECTION('center_axis',(0.,0.,1.));
#5649=DIRECTION('ref_axis',(1.,0.,0.));
#5650=DIRECTION('center_axis',(0.,0.,1.));
#5651=DIRECTION('ref_axis',(1.,0.,0.));
#5652=DIRECTION('axis',(0.,0.,1.));
#5653=DIRECTION('refdir',(1.,0.,0.));
#5654=DIRECTION('center_axis',(0.,0.,1.));
#5655=DIRECTION('ref_axis',(1.,0.,0.));
#5656=DIRECTION('center_axis',(0.,0.,1.));
#5657=DIRECTION('ref_axis',(1.,0.,0.));
#5658=DIRECTION('',(0.,0.,-1.));
#5659=DIRECTION('center_axis',(0.,0.,1.));
#5660=DIRECTION('ref_axis',(1.,0.,0.));
#5661=DIRECTION('center_axis',(0.,0.,1.));
#5662=DIRECTION('ref_axis',(1.,0.,0.));
#5663=DIRECTION('center_axis',(0.,0.,1.));
#5664=DIRECTION('ref_axis',(1.,0.,0.));
#5665=DIRECTION('axis',(0.,0.,1.));
#5666=DIRECTION('refdir',(1.,0.,0.));
#5667=DIRECTION('center_axis',(0.,0.,1.));
#5668=DIRECTION('ref_axis',(1.,0.,0.));
#5669=DIRECTION('center_axis',(0.,0.,1.));
#5670=DIRECTION('ref_axis',(1.,0.,0.));
#5671=DIRECTION('',(0.,0.,-1.));
#5672=DIRECTION('center_axis',(0.,0.,1.));
#5673=DIRECTION('ref_axis',(1.,0.,0.));
#5674=DIRECTION('center_axis',(0.,0.,1.));
#5675=DIRECTION('ref_axis',(1.,0.,0.));
#5676=DIRECTION('center_axis',(0.,0.,1.));
#5677=DIRECTION('ref_axis',(1.,0.,0.));
#5678=DIRECTION('axis',(0.,0.,1.));
#5679=DIRECTION('refdir',(1.,0.,0.));
#5680=DIRECTION('center_axis',(0.,0.,1.));
#5681=DIRECTION('ref_axis',(1.,0.,0.));
#5682=DIRECTION('center_axis',(0.,0.,1.));
#5683=DIRECTION('ref_axis',(1.,0.,0.));
#5684=DIRECTION('',(0.,0.,-1.));
#5685=DIRECTION('center_axis',(0.,0.,1.));
#5686=DIRECTION('ref_axis',(1.,0.,0.));
#5687=DIRECTION('center_axis',(0.,0.,1.));
#5688=DIRECTION('ref_axis',(1.,0.,0.));
#5689=DIRECTION('center_axis',(0.,0.,1.));
#5690=DIRECTION('ref_axis',(1.,0.,0.));
#5691=DIRECTION('axis',(0.,0.,1.));
#5692=DIRECTION('refdir',(1.,0.,0.));
#5693=DIRECTION('center_axis',(0.,0.,1.));
#5694=DIRECTION('ref_axis',(1.,0.,0.));
#5695=DIRECTION('center_axis',(0.,0.,1.));
#5696=DIRECTION('ref_axis',(1.,0.,0.));
#5697=DIRECTION('',(0.,0.,-1.));
#5698=DIRECTION('center_axis',(0.,0.,1.));
#5699=DIRECTION('ref_axis',(1.,0.,0.));
#5700=DIRECTION('center_axis',(0.,0.,1.));
#5701=DIRECTION('ref_axis',(1.,0.,0.));
#5702=DIRECTION('center_axis',(0.,0.,1.));
#5703=DIRECTION('ref_axis',(1.,0.,0.));
#5704=DIRECTION('axis',(0.,0.,1.));
#5705=DIRECTION('refdir',(1.,0.,0.));
#5706=DIRECTION('center_axis',(0.,0.,1.));
#5707=DIRECTION('ref_axis',(1.,0.,0.));
#5708=DIRECTION('center_axis',(0.,0.,1.));
#5709=DIRECTION('ref_axis',(1.,0.,0.));
#5710=DIRECTION('',(0.,0.,1.));
#5711=DIRECTION('center_axis',(0.,0.,-1.));
#5712=DIRECTION('ref_axis',(1.,0.,0.));
#5713=DIRECTION('center_axis',(0.,0.,1.));
#5714=DIRECTION('ref_axis',(1.,0.,0.));
#5715=DIRECTION('center_axis',(0.,0.,1.));
#5716=DIRECTION('ref_axis',(1.,0.,0.));
#5717=DIRECTION('',(0.,0.,1.));
#5718=DIRECTION('center_axis',(0.,0.,-1.));
#5719=DIRECTION('ref_axis',(1.,0.,0.));
#5720=DIRECTION('center_axis',(0.,0.,1.));
#5721=DIRECTION('ref_axis',(1.,0.,0.));
#5722=DIRECTION('center_axis',(0.,0.,1.));
#5723=DIRECTION('ref_axis',(1.,0.,0.));
#5724=DIRECTION('',(0.,0.,1.));
#5725=DIRECTION('center_axis',(0.,0.,-1.));
#5726=DIRECTION('ref_axis',(1.,0.,0.));
#5727=DIRECTION('center_axis',(0.,0.,1.));
#5728=DIRECTION('ref_axis',(1.,0.,0.));
#5729=DIRECTION('center_axis',(0.,0.,1.));
#5730=DIRECTION('ref_axis',(1.,0.,0.));
#5731=DIRECTION('',(0.,0.,1.));
#5732=DIRECTION('center_axis',(0.,0.,-1.));
#5733=DIRECTION('ref_axis',(1.,0.,0.));
#5734=DIRECTION('center_axis',(0.,0.,1.));
#5735=DIRECTION('ref_axis',(1.,0.,0.));
#5736=DIRECTION('center_axis',(0.,0.,1.));
#5737=DIRECTION('ref_axis',(1.,0.,0.));
#5738=DIRECTION('center_axis',(0.,0.,1.));
#5739=DIRECTION('ref_axis',(1.,0.,0.));
#5740=DIRECTION('center_axis',(0.,0.,1.));
#5741=DIRECTION('ref_axis',(1.,0.,0.));
#5742=DIRECTION('center_axis',(0.,0.,1.));
#5743=DIRECTION('ref_axis',(1.,0.,0.));
#5744=DIRECTION('center_axis',(0.,0.,-1.));
#5745=DIRECTION('ref_axis',(1.,0.,0.));
#5746=DIRECTION('center_axis',(0.,0.,1.));
#5747=DIRECTION('ref_axis',(1.,0.,0.));
#5748=DIRECTION('',(0.,0.,-1.));
#5749=DIRECTION('center_axis',(0.,0.,1.));
#5750=DIRECTION('ref_axis',(1.,0.,0.));
#5751=DIRECTION('',(0.,0.,-1.));
#5752=DIRECTION('center_axis',(0.,0.,1.));
#5753=DIRECTION('ref_axis',(1.,0.,0.));
#5754=DIRECTION('center_axis',(0.,0.,1.));
#5755=DIRECTION('ref_axis',(1.,0.,0.));
#5756=DIRECTION('center_axis',(0.,0.,1.));
#5757=DIRECTION('ref_axis',(1.,0.,0.));
#5758=DIRECTION('center_axis',(0.,0.,1.));
#5759=DIRECTION('ref_axis',(1.,0.,0.));
#5760=DIRECTION('',(0.,0.,-1.));
#5761=DIRECTION('center_axis',(0.,0.,1.));
#5762=DIRECTION('ref_axis',(1.,0.,0.));
#5763=DIRECTION('center_axis',(0.,0.,1.));
#5764=DIRECTION('ref_axis',(1.,0.,0.));
#5765=DIRECTION('center_axis',(0.,0.,1.));
#5766=DIRECTION('ref_axis',(1.,0.,0.));
#5767=DIRECTION('',(0.,0.,-1.));
#5768=DIRECTION('center_axis',(0.,0.,1.));
#5769=DIRECTION('ref_axis',(1.,0.,0.));
#5770=DIRECTION('center_axis',(0.,0.,1.));
#5771=DIRECTION('ref_axis',(1.,0.,0.));
#5772=DIRECTION('axis',(0.,0.,1.));
#5773=DIRECTION('refdir',(1.,0.,0.));
#5774=DIRECTION('center_axis',(0.,0.,1.));
#5775=DIRECTION('ref_axis',(1.,0.,0.));
#5776=DIRECTION('center_axis',(0.,0.,-1.));
#5777=DIRECTION('ref_axis',(1.,0.,0.));
#5778=DIRECTION('',(0.,0.,-1.));
#5779=DIRECTION('center_axis',(0.,0.,-1.));
#5780=DIRECTION('ref_axis',(1.,0.,0.));
#5781=DIRECTION('center_axis',(0.,0.,1.));
#5782=DIRECTION('ref_axis',(1.,0.,0.));
#5783=DIRECTION('center_axis',(0.,0.,1.));
#5784=DIRECTION('ref_axis',(1.,0.,0.));
#5785=DIRECTION('',(0.,0.,-1.));
#5786=DIRECTION('center_axis',(0.,0.,1.));
#5787=DIRECTION('ref_axis',(1.,0.,0.));
#5788=DIRECTION('center_axis',(0.,0.,1.));
#5789=DIRECTION('ref_axis',(1.,0.,0.));
#5790=DIRECTION('center_axis',(0.,0.,1.));
#5791=DIRECTION('ref_axis',(1.,0.,0.));
#5792=DIRECTION('axis',(0.,0.,1.));
#5793=DIRECTION('refdir',(1.,0.,0.));
#5794=DIRECTION('center_axis',(1.,0.,0.));
#5795=DIRECTION('ref_axis',(0.,0.,-1.));
#5796=DIRECTION('',(0.,0.,1.));
#5797=DIRECTION('center_axis',(1.,0.,0.));
#5798=DIRECTION('ref_axis',(0.,0.,-1.));
#5799=DIRECTION('center_axis',(1.,0.,0.));
#5800=DIRECTION('ref_axis',(0.,0.,-1.));
#5801=DIRECTION('center_axis',(1.,0.,0.));
#5802=DIRECTION('ref_axis',(0.,0.,-1.));
#5803=DIRECTION('',(1.,0.,0.));
#5804=DIRECTION('center_axis',(1.,0.,0.));
#5805=DIRECTION('ref_axis',(0.,0.,-1.));
#5806=DIRECTION('',(0.,0.,-1.));
#5807=DIRECTION('center_axis',(0.,0.,1.));
#5808=DIRECTION('ref_axis',(1.,0.,0.));
#5809=DIRECTION('center_axis',(0.,0.,-1.));
#5810=DIRECTION('ref_axis',(1.,0.,0.));
#5811=DIRECTION('',(0.,0.,-1.));
#5812=DIRECTION('center_axis',(0.,0.,-1.));
#5813=DIRECTION('ref_axis',(1.,0.,0.));
#5814=DIRECTION('center_axis',(0.,0.,1.));
#5815=DIRECTION('ref_axis',(1.,0.,0.));
#5816=DIRECTION('center_axis',(0.,0.,1.));
#5817=DIRECTION('ref_axis',(1.,0.,0.));
#5818=DIRECTION('',(0.,0.,-1.));
#5819=DIRECTION('center_axis',(0.,0.,1.));
#5820=DIRECTION('ref_axis',(1.,0.,0.));
#5821=DIRECTION('center_axis',(0.,0.,1.));
#5822=DIRECTION('ref_axis',(1.,0.,0.));
#5823=DIRECTION('center_axis',(0.,0.,1.));
#5824=DIRECTION('ref_axis',(1.,0.,0.));
#5825=DIRECTION('axis',(0.,0.,1.));
#5826=DIRECTION('refdir',(1.,0.,0.));
#5827=DIRECTION('center_axis',(0.,0.,1.));
#5828=DIRECTION('ref_axis',(1.,0.,0.));
#5829=DIRECTION('center_axis',(0.,0.,1.));
#5830=DIRECTION('ref_axis',(1.,0.,0.));
#5831=DIRECTION('',(0.,0.,1.));
#5832=DIRECTION('center_axis',(0.,0.,-1.));
#5833=DIRECTION('ref_axis',(1.,0.,0.));
#5834=DIRECTION('center_axis',(0.,0.,1.));
#5835=DIRECTION('ref_axis',(1.,0.,0.));
#5836=DIRECTION('center_axis',(0.,0.,1.));
#5837=DIRECTION('ref_axis',(1.,0.,0.));
#5838=DIRECTION('',(0.,0.,1.));
#5839=DIRECTION('center_axis',(0.,0.,-1.));
#5840=DIRECTION('ref_axis',(1.,0.,0.));
#5841=DIRECTION('center_axis',(0.,0.,1.));
#5842=DIRECTION('ref_axis',(1.,0.,0.));
#5843=DIRECTION('center_axis',(0.,0.,1.));
#5844=DIRECTION('ref_axis',(1.,0.,0.));
#5845=DIRECTION('',(0.,0.,1.));
#5846=DIRECTION('center_axis',(0.,0.,-1.));
#5847=DIRECTION('ref_axis',(1.,0.,0.));
#5848=DIRECTION('center_axis',(0.,0.,1.));
#5849=DIRECTION('ref_axis',(1.,0.,0.));
#5850=DIRECTION('center_axis',(0.,0.,1.));
#5851=DIRECTION('ref_axis',(1.,0.,0.));
#5852=DIRECTION('center_axis',(0.,0.,1.));
#5853=DIRECTION('ref_axis',(1.,0.,0.));
#5854=DIRECTION('',(0.,0.,-1.));
#5855=DIRECTION('center_axis',(0.,0.,-1.));
#5856=DIRECTION('ref_axis',(1.,0.,0.));
#5857=DIRECTION('center_axis',(0.,0.,1.));
#5858=DIRECTION('ref_axis',(1.,0.,0.));
#5859=DIRECTION('center_axis',(0.,0.,1.));
#5860=DIRECTION('ref_axis',(1.,0.,0.));
#5861=DIRECTION('',(0.,0.,-1.));
#5862=DIRECTION('center_axis',(0.,0.,1.));
#5863=DIRECTION('ref_axis',(1.,0.,0.));
#5864=DIRECTION('center_axis',(0.,0.,1.));
#5865=DIRECTION('ref_axis',(1.,0.,0.));
#5866=DIRECTION('center_axis',(0.,0.,1.));
#5867=DIRECTION('ref_axis',(1.,0.,0.));
#5868=DIRECTION('axis',(0.,0.,1.));
#5869=DIRECTION('refdir',(1.,0.,0.));
#5870=DIRECTION('center_axis',(0.,0.,1.));
#5871=DIRECTION('ref_axis',(1.,0.,0.));
#5872=DIRECTION('center_axis',(0.,0.,-1.));
#5873=DIRECTION('ref_axis',(1.,0.,0.));
#5874=DIRECTION('',(0.,0.,-1.));
#5875=DIRECTION('center_axis',(0.,0.,-1.));
#5876=DIRECTION('ref_axis',(1.,0.,0.));
#5877=DIRECTION('center_axis',(0.,0.,1.));
#5878=DIRECTION('ref_axis',(1.,0.,0.));
#5879=DIRECTION('center_axis',(0.,0.,1.));
#5880=DIRECTION('ref_axis',(1.,0.,0.));
#5881=DIRECTION('center_axis',(0.,0.,1.));
#5882=DIRECTION('ref_axis',(1.,0.,0.));
#5883=DIRECTION('',(0.,0.,-1.));
#5884=DIRECTION('center_axis',(0.,0.,-1.));
#5885=DIRECTION('ref_axis',(1.,0.,0.));
#5886=DIRECTION('center_axis',(0.,0.,1.));
#5887=DIRECTION('ref_axis',(1.,0.,0.));
#5888=DIRECTION('center_axis',(0.,0.,1.));
#5889=DIRECTION('ref_axis',(1.,0.,0.));
#5890=DIRECTION('',(0.,0.,-1.));
#5891=DIRECTION('center_axis',(0.,0.,1.));
#5892=DIRECTION('ref_axis',(1.,0.,0.));
#5893=DIRECTION('center_axis',(0.,0.,1.));
#5894=DIRECTION('ref_axis',(1.,0.,0.));
#5895=DIRECTION('center_axis',(0.,0.,1.));
#5896=DIRECTION('ref_axis',(1.,0.,0.));
#5897=DIRECTION('axis',(0.,0.,1.));
#5898=DIRECTION('refdir',(1.,0.,0.));
#5899=DIRECTION('center_axis',(-0.000132267085706657,0.981242764302753,
0.192776087751852));
#5900=DIRECTION('ref_axis',(2.59853443172113E-5,-0.192776086000499,0.981242773217255));
#5901=DIRECTION('center_axis',(0.000132265595059966,0.981242764048193,0.192776089048605));
#5902=DIRECTION('ref_axis',(-0.796598144949105,0.116638308439033,-0.593149981428075));
#5903=DIRECTION('center_axis',(0.000132265595059966,0.981242764048193,0.192776089048605));
#5904=DIRECTION('ref_axis',(-0.796598144949105,0.116638308439033,-0.593149981428075));
#5905=DIRECTION('center_axis',(-0.000132267085706657,0.981242764302753,
0.192776087751852));
#5906=DIRECTION('ref_axis',(2.59853443172113E-5,-0.192776086000499,0.981242773217256));
#5907=DIRECTION('axis',(0.,0.,1.));
#5908=DIRECTION('refdir',(1.,0.,0.));
#5909=DIRECTION('center_axis',(0.,1.,0.));
#5910=DIRECTION('ref_axis',(1.,0.,0.));
#5911=DIRECTION('center_axis',(0.,-1.,0.));
#5912=DIRECTION('ref_axis',(1.,0.,0.));
#5913=DIRECTION('',(0.,-1.,0.));
#5914=DIRECTION('center_axis',(0.,-1.,0.));
#5915=DIRECTION('ref_axis',(1.,0.,0.));
#5916=DIRECTION('center_axis',(0.,1.,0.));
#5917=DIRECTION('ref_axis',(1.,0.,0.));
#5918=DIRECTION('center_axis',(0.,1.,0.));
#5919=DIRECTION('ref_axis',(1.,0.,0.));
#5920=DIRECTION('',(0.,-1.,0.));
#5921=DIRECTION('center_axis',(0.,1.,0.));
#5922=DIRECTION('ref_axis',(1.,0.,0.));
#5923=DIRECTION('center_axis',(0.,1.,0.));
#5924=DIRECTION('ref_axis',(1.,0.,0.));
#5925=DIRECTION('center_axis',(0.,1.,0.));
#5926=DIRECTION('ref_axis',(1.,0.,0.));
#5927=DIRECTION('axis',(0.,0.,1.));
#5928=DIRECTION('refdir',(1.,0.,0.));
#5929=DIRECTION('center_axis',(0.866025403784439,0.,-0.5));
#5930=DIRECTION('ref_axis',(0.5,0.,0.866025403784439));
#5931=DIRECTION('',(-0.5,0.,-0.866025403784439));
#5932=DIRECTION('',(0.,-1.,0.));
#5933=DIRECTION('',(0.5,0.,0.866025403784439));
#5934=DIRECTION('',(0.,-1.,0.));
#5935=DIRECTION('center_axis',(1.92296268638356E-16,0.,-1.));
#5936=DIRECTION('ref_axis',(1.,0.,1.92296268638356E-16));
#5937=DIRECTION('',(-1.,0.,-1.92296268638356E-16));
#5938=DIRECTION('',(0.,-1.,0.));
#5939=DIRECTION('',(1.,0.,1.92296268638356E-16));
#5940=DIRECTION('center_axis',(-0.866025403784439,0.,-0.5));
#5941=DIRECTION('ref_axis',(0.5,0.,-0.866025403784439));
#5942=DIRECTION('',(-0.5,0.,0.866025403784438));
#5943=DIRECTION('',(0.,-1.,0.));
#5944=DIRECTION('',(0.5,0.,-0.866025403784438));
#5945=DIRECTION('center_axis',(-0.866025403784439,0.,0.5));
#5946=DIRECTION('ref_axis',(-0.5,0.,-0.866025403784439));
#5947=DIRECTION('',(0.5,0.,0.866025403784439));
#5948=DIRECTION('',(0.,-1.,0.));
#5949=DIRECTION('',(-0.5,0.,-0.866025403784439));
#5950=DIRECTION('center_axis',(-1.92296268638356E-16,0.,1.));
#5951=DIRECTION('ref_axis',(-1.,0.,-1.92296268638356E-16));
#5952=DIRECTION('',(1.,0.,1.92296268638356E-16));
#5953=DIRECTION('',(0.,-1.,0.));
#5954=DIRECTION('',(-1.,0.,-1.92296268638356E-16));
#5955=DIRECTION('center_axis',(0.866025403784439,0.,0.5));
#5956=DIRECTION('ref_axis',(-0.5,0.,0.866025403784439));
#5957=DIRECTION('',(0.5,0.,-0.866025403784439));
#5958=DIRECTION('',(-0.5,0.,0.866025403784439));
#5959=DIRECTION('center_axis',(0.,1.,0.));
#5960=DIRECTION('ref_axis',(1.,0.,0.));
#5961=DIRECTION('center_axis',(0.,-1.,0.));
#5962=DIRECTION('ref_axis',(0.,0.,-1.));
#5963=DIRECTION('center_axis',(0.,1.,0.));
#5964=DIRECTION('ref_axis',(1.,0.,0.));
#5965=DIRECTION('center_axis',(0.,1.,0.));
#5966=DIRECTION('ref_axis',(1.,0.,0.));
#5967=DIRECTION('center_axis',(0.,1.,0.));
#5968=DIRECTION('ref_axis',(0.,0.,1.));
#5969=DIRECTION('center_axis',(0.,-1.,0.));
#5970=DIRECTION('ref_axis',(1.,0.,0.));
#5971=DIRECTION('center_axis',(0.,-1.,0.));
#5972=DIRECTION('ref_axis',(1.,0.,0.));
#5973=DIRECTION('center_axis',(0.,-1.,0.));
#5974=DIRECTION('ref_axis',(1.,0.,0.));
#5975=DIRECTION('',(0.707106781186548,0.707106781186547,8.65956056235494E-17));
#5976=DIRECTION('center_axis',(0.,-1.,0.));
#5977=DIRECTION('ref_axis',(1.,0.,0.));
#5978=DIRECTION('center_axis',(0.,-1.,0.));
#5979=DIRECTION('ref_axis',(1.,0.,0.));
#5980=DIRECTION('',(0.,1.,0.));
#5981=DIRECTION('center_axis',(0.,1.,0.));
#5982=DIRECTION('ref_axis',(1.,0.,0.));
#5983=DIRECTION('center_axis',(0.,-1.,0.));
#5984=DIRECTION('ref_axis',(1.,0.,0.));
#5985=DIRECTION('',(-0.707106781186547,0.707106781186548,-8.65956056235493E-17));
#5986=DIRECTION('center_axis',(0.,-1.,0.));
#5987=DIRECTION('ref_axis',(0.,0.,-1.));
#5988=DIRECTION('center_axis',(0.,-1.,0.));
#5989=DIRECTION('ref_axis',(1.,0.,0.));
#5990=DIRECTION('center_axis',(0.,1.,0.));
#5991=DIRECTION('ref_axis',(1.,0.,0.));
#5992=DIRECTION('center_axis',(0.,1.,0.));
#5993=DIRECTION('ref_axis',(1.,0.,0.));
#5994=DIRECTION('',(-0.447213595499958,0.894427190999916,-5.47678698264203E-17));
#5995=DIRECTION('center_axis',(0.,-1.,0.));
#5996=DIRECTION('ref_axis',(1.,0.,0.));
#5997=DIRECTION('',(0.,1.,0.));
#5998=DIRECTION('axis',(0.,0.,1.));
#5999=DIRECTION('refdir',(1.,0.,0.));
#6000=DIRECTION('axis',(0.,0.,1.));
#6001=DIRECTION('refdir',(1.,0.,0.));
#6002=DIRECTION('center_axis',(0.,-1.,0.));
#6003=DIRECTION('ref_axis',(0.,0.,-1.));
#6004=DIRECTION('center_axis',(0.,-1.,0.));
#6005=DIRECTION('ref_axis',(1.,0.,0.));
#6006=DIRECTION('center_axis',(0.,-1.,0.));
#6007=DIRECTION('ref_axis',(1.,0.,0.));
#6008=DIRECTION('center_axis',(1.,0.,1.22464679914735E-16));
#6009=DIRECTION('ref_axis',(-1.22464679914735E-16,0.,1.));
#6010=DIRECTION('center_axis',(0.,1.,0.));
#6011=DIRECTION('ref_axis',(1.,0.,0.));
#6012=DIRECTION('center_axis',(0.,1.,0.));
#6013=DIRECTION('ref_axis',(1.,0.,0.));
#6014=DIRECTION('center_axis',(0.,-1.,0.));
#6015=DIRECTION('ref_axis',(1.,0.,0.));
#6016=DIRECTION('',(0.,1.,0.));
#6017=DIRECTION('center_axis',(0.,-1.,0.));
#6018=DIRECTION('ref_axis',(1.,0.,0.));
#6019=DIRECTION('center_axis',(0.,-1.,0.));
#6020=DIRECTION('ref_axis',(1.,0.,0.));
#6021=DIRECTION('center_axis',(0.,-1.,0.));
#6022=DIRECTION('ref_axis',(1.,0.,0.));
#6023=DIRECTION('',(0.,1.,0.));
#6024=DIRECTION('center_axis',(0.,-1.,0.));
#6025=DIRECTION('ref_axis',(1.,0.,0.));
#6026=DIRECTION('center_axis',(0.,1.,0.));
#6027=DIRECTION('ref_axis',(1.,0.,0.));
#6028=DIRECTION('',(-0.707106781186548,0.707106781186547,-8.65956056235494E-17));
#6029=DIRECTION('center_axis',(0.,-1.,0.));
#6030=DIRECTION('ref_axis',(1.,0.,0.));
#6031=DIRECTION('center_axis',(0.,1.,0.));
#6032=DIRECTION('ref_axis',(0.,0.,1.));
#6033=DIRECTION('center_axis',(0.,-1.,0.));
#6034=DIRECTION('ref_axis',(1.,0.,0.));
#6035=DIRECTION('center_axis',(0.,-1.,0.));
#6036=DIRECTION('ref_axis',(1.,0.,0.));
#6037=DIRECTION('',(0.,1.,0.));
#6038=DIRECTION('center_axis',(0.,-1.,0.));
#6039=DIRECTION('ref_axis',(0.,0.,-1.));
#6040=DIRECTION('center_axis',(0.,-1.,0.));
#6041=DIRECTION('ref_axis',(1.,0.,0.));
#6042=DIRECTION('center_axis',(0.,-1.,0.));
#6043=DIRECTION('ref_axis',(1.,0.,0.));
#6044=DIRECTION('',(0.707106781186548,0.707106781186547,8.65956056235494E-17));
#6045=DIRECTION('axis',(0.,0.,1.));
#6046=DIRECTION('refdir',(1.,0.,0.));
#6047=DIRECTION('center_axis',(0.,-1.,0.));
#6048=DIRECTION('ref_axis',(0.,0.,-1.));
#6049=DIRECTION('center_axis',(0.,-1.,0.));
#6050=DIRECTION('ref_axis',(1.,0.,0.));
#6051=DIRECTION('center_axis',(0.,-1.,0.));
#6052=DIRECTION('ref_axis',(1.,0.,0.));
#6053=DIRECTION('center_axis',(1.,0.,1.22464679914735E-16));
#6054=DIRECTION('ref_axis',(-1.22464679914735E-16,0.,1.));
#6055=DIRECTION('center_axis',(0.,1.,0.));
#6056=DIRECTION('ref_axis',(1.,0.,0.));
#6057=DIRECTION('center_axis',(0.,1.,0.));
#6058=DIRECTION('ref_axis',(1.,0.,0.));
#6059=DIRECTION('center_axis',(0.,-1.,0.));
#6060=DIRECTION('ref_axis',(1.,0.,0.));
#6061=DIRECTION('center_axis',(0.,-1.,0.));
#6062=DIRECTION('ref_axis',(1.,0.,0.));
#6063=DIRECTION('',(0.,1.,0.));
#6064=DIRECTION('center_axis',(0.,1.,0.));
#6065=DIRECTION('ref_axis',(0.,0.,1.));
#6066=DIRECTION('center_axis',(0.,-1.,0.));
#6067=DIRECTION('ref_axis',(1.,0.,0.));
#6068=DIRECTION('center_axis',(0.,-1.,0.));
#6069=DIRECTION('ref_axis',(1.,0.,0.));
#6070=DIRECTION('center_axis',(0.,-1.,0.));
#6071=DIRECTION('ref_axis',(1.,0.,0.));
#6072=DIRECTION('center_axis',(0.,-1.,0.));
#6073=DIRECTION('ref_axis',(1.,0.,0.));
#6074=DIRECTION('',(0.707106781186548,0.707106781186547,8.65956056235494E-17));
#6075=DIRECTION('center_axis',(0.,-1.,0.));
#6076=DIRECTION('ref_axis',(1.,0.,0.));
#6077=DIRECTION('center_axis',(0.,-1.,0.));
#6078=DIRECTION('ref_axis',(1.,0.,0.));
#6079=DIRECTION('',(0.,1.,0.));
#6080=DIRECTION('center_axis',(0.,1.,0.));
#6081=DIRECTION('ref_axis',(1.,0.,0.));
#6082=DIRECTION('center_axis',(0.,-1.,0.));
#6083=DIRECTION('ref_axis',(1.,0.,0.));
#6084=DIRECTION('',(-0.707106781186548,0.707106781186547,-8.65956056235494E-17));
#6085=DIRECTION('center_axis',(0.,-1.,0.));
#6086=DIRECTION('ref_axis',(0.,0.,-1.));
#6087=DIRECTION('center_axis',(0.,-1.,0.));
#6088=DIRECTION('ref_axis',(1.,0.,0.));
#6089=DIRECTION('',(0.,1.,0.));
#6090=DIRECTION('axis',(0.,0.,1.));
#6091=DIRECTION('refdir',(1.,0.,0.));
#6092=DIRECTION('center_axis',(0.,0.,1.));
#6093=DIRECTION('ref_axis',(1.,0.,0.));
#6094=DIRECTION('center_axis',(1.22464679914735E-16,-1.,0.));
#6095=DIRECTION('ref_axis',(-1.,-1.22464679914735E-16,0.));
#6096=DIRECTION('center_axis',(0.642787609686539,0.,0.766044443118978));
#6097=DIRECTION('ref_axis',(0.766044443118978,0.,-0.642787609686539));
#6098=DIRECTION('center_axis',(9.38133875270273E-17,-1.,-7.87187788734199E-17));
#6099=DIRECTION('ref_axis',(-0.766044443118978,-1.22464679914735E-16,0.642787609686539));
#6100=DIRECTION('center_axis',(0.984807753012208,0.,0.173648177666931));
#6101=DIRECTION('ref_axis',(0.17364817766693,0.,-0.984807753012208));
#6102=DIRECTION('center_axis',(2.12657684957577E-17,-1.,-1.2060416625019E-16));
#6103=DIRECTION('ref_axis',(-0.17364817766693,-1.22464679914735E-16,0.984807753012208));
#6104=DIRECTION('center_axis',(0.866025403784439,0.,-0.5));
#6105=DIRECTION('ref_axis',(-0.5,0.,-0.866025403784439));
#6106=DIRECTION('center_axis',(-6.12323399573676E-17,-1.,-1.06057523872491E-16));
#6107=DIRECTION('ref_axis',(0.5,-1.22464679914735E-16,0.866025403784439));
#6108=DIRECTION('center_axis',(0.342020143325669,0.,-0.939692620785908));
#6109=DIRECTION('ref_axis',(-0.939692620785908,0.,-0.342020143325669));
#6110=DIRECTION('center_axis',(-1.15079156022785E-16,-1.,-4.18853873767699E-17));
#6111=DIRECTION('ref_axis',(0.939692620785908,-1.22464679914735E-16,0.342020143325669));
#6112=DIRECTION('center_axis',(-0.342020143325669,0.,-0.939692620785908));
#6113=DIRECTION('ref_axis',(-0.939692620785909,0.,0.342020143325669));
#6114=DIRECTION('center_axis',(-1.15079156022785E-16,-1.,4.18853873767699E-17));
#6115=DIRECTION('ref_axis',(0.939692620785908,-1.22464679914735E-16,-0.342020143325669));
#6116=DIRECTION('center_axis',(-0.866025403784438,0.,-0.5));
#6117=DIRECTION('ref_axis',(-0.5,0.,0.866025403784438));
#6118=DIRECTION('center_axis',(-6.12323399573677E-17,-1.,1.06057523872491E-16));
#6119=DIRECTION('ref_axis',(0.5,-1.22464679914735E-16,-0.866025403784438));
#6120=DIRECTION('center_axis',(-0.984807753012208,0.,0.17364817766693));
#6121=DIRECTION('ref_axis',(0.17364817766693,0.,0.984807753012208));
#6122=DIRECTION('center_axis',(2.12657684957577E-17,-1.,1.2060416625019E-16));
#6123=DIRECTION('ref_axis',(-0.17364817766693,-1.22464679914735E-16,-0.984807753012208));
#6124=DIRECTION('center_axis',(-0.64278760968654,0.,0.766044443118978));
#6125=DIRECTION('ref_axis',(0.766044443118978,0.,0.64278760968654));
#6126=DIRECTION('center_axis',(9.38133875270273E-17,-1.,7.87187788734199E-17));
#6127=DIRECTION('ref_axis',(-0.766044443118978,-1.22464679914735E-16,-0.64278760968654));
#6128=DIRECTION('axis',(0.,0.,1.));
#6129=DIRECTION('refdir',(1.,0.,0.));
#6130=DIRECTION('center_axis',(0.,0.,1.));
#6131=DIRECTION('ref_axis',(1.,0.,0.));
#6132=DIRECTION('center_axis',(0.,-1.,0.));
#6133=DIRECTION('ref_axis',(0.,0.,-1.));
#6134=DIRECTION('center_axis',(0.,-1.,0.));
#6135=DIRECTION('ref_axis',(0.,0.,-1.));
#6136=DIRECTION('center_axis',(0.,1.,0.));
#6137=DIRECTION('ref_axis',(1.,0.,0.));
#6138=DIRECTION('center_axis',(0.,1.,0.));
#6139=DIRECTION('ref_axis',(1.,0.,0.));
#6140=DIRECTION('center_axis',(0.,1.,0.));
#6141=DIRECTION('ref_axis',(1.,0.,0.));
#6142=DIRECTION('center_axis',(0.,1.,0.));
#6143=DIRECTION('ref_axis',(1.,0.,0.));
#6144=DIRECTION('center_axis',(0.,1.,0.));
#6145=DIRECTION('ref_axis',(1.,0.,0.));
#6146=DIRECTION('',(0.,-1.,0.));
#6147=DIRECTION('center_axis',(0.,-1.,0.));
#6148=DIRECTION('ref_axis',(1.,0.,0.));
#6149=DIRECTION('center_axis',(0.,1.,0.));
#6150=DIRECTION('ref_axis',(1.,0.,0.));
#6151=DIRECTION('center_axis',(0.,1.,0.));
#6152=DIRECTION('ref_axis',(1.,0.,0.));
#6153=DIRECTION('center_axis',(0.,1.,0.));
#6154=DIRECTION('ref_axis',(1.,0.,0.));
#6155=DIRECTION('center_axis',(0.,1.,0.));
#6156=DIRECTION('ref_axis',(1.,0.,0.));
#6157=DIRECTION('center_axis',(0.,1.,0.));
#6158=DIRECTION('ref_axis',(1.,0.,0.));
#6159=DIRECTION('center_axis',(0.,1.,0.));
#6160=DIRECTION('ref_axis',(1.,0.,0.));
#6161=DIRECTION('center_axis',(0.,1.,0.));
#6162=DIRECTION('ref_axis',(1.,0.,0.));
#6163=DIRECTION('center_axis',(0.,-1.,0.));
#6164=DIRECTION('ref_axis',(1.,0.,0.));
#6165=DIRECTION('center_axis',(0.,-1.,0.));
#6166=DIRECTION('ref_axis',(0.,0.,-1.));
#6167=DIRECTION('center_axis',(0.,0.,1.));
#6168=DIRECTION('ref_axis',(1.,0.,0.));
#6169=DIRECTION('center_axis',(0.,-1.,0.));
#6170=DIRECTION('ref_axis',(0.,0.,-1.));
#6171=DIRECTION('center_axis',(0.,1.,0.));
#6172=DIRECTION('ref_axis',(1.,0.,0.));
#6173=DIRECTION('center_axis',(0.,-1.,0.));
#6174=DIRECTION('ref_axis',(1.,0.,0.));
#6175=DIRECTION('center_axis',(0.,-1.,0.));
#6176=DIRECTION('ref_axis',(0.,0.,-1.));
#6177=DIRECTION('center_axis',(0.,0.,1.));
#6178=DIRECTION('ref_axis',(1.,0.,0.));
#6179=DIRECTION('center_axis',(0.,-1.,0.));
#6180=DIRECTION('ref_axis',(0.,0.,-1.));
#6181=DIRECTION('center_axis',(0.,1.,0.));
#6182=DIRECTION('ref_axis',(1.,0.,0.));
#6183=DIRECTION('center_axis',(0.,-1.,0.));
#6184=DIRECTION('ref_axis',(1.,0.,0.));
#6185=DIRECTION('center_axis',(0.,-1.,0.));
#6186=DIRECTION('ref_axis',(0.,0.,-1.));
#6187=DIRECTION('center_axis',(0.,0.,1.));
#6188=DIRECTION('ref_axis',(1.,0.,0.));
#6189=DIRECTION('center_axis',(0.,-1.,0.));
#6190=DIRECTION('ref_axis',(0.,0.,-1.));
#6191=DIRECTION('center_axis',(0.,1.,0.));
#6192=DIRECTION('ref_axis',(1.,0.,0.));
#6193=DIRECTION('center_axis',(0.,-1.,0.));
#6194=DIRECTION('ref_axis',(1.,0.,0.));
#6195=DIRECTION('center_axis',(0.,-1.,0.));
#6196=DIRECTION('ref_axis',(1.,0.,0.));
#6197=DIRECTION('center_axis',(0.,-1.,0.));
#6198=DIRECTION('ref_axis',(0.,0.,-1.));
#6199=DIRECTION('center_axis',(0.,0.,1.));
#6200=DIRECTION('ref_axis',(1.,0.,0.));
#6201=DIRECTION('center_axis',(0.,-1.,0.));
#6202=DIRECTION('ref_axis',(0.,0.,-1.));
#6203=DIRECTION('center_axis',(0.,1.,0.));
#6204=DIRECTION('ref_axis',(1.,0.,0.));
#6205=DIRECTION('center_axis',(0.,-1.,0.));
#6206=DIRECTION('ref_axis',(1.,0.,0.));
#6207=DIRECTION('center_axis',(0.,-1.,0.));
#6208=DIRECTION('ref_axis',(0.,0.,-1.));
#6209=DIRECTION('center_axis',(0.,0.,1.));
#6210=DIRECTION('ref_axis',(1.,0.,0.));
#6211=DIRECTION('center_axis',(0.,-1.,0.));
#6212=DIRECTION('ref_axis',(0.,0.,-1.));
#6213=DIRECTION('center_axis',(0.,1.,0.));
#6214=DIRECTION('ref_axis',(1.,0.,0.));
#6215=DIRECTION('center_axis',(0.,-1.,0.));
#6216=DIRECTION('ref_axis',(1.,0.,0.));
#6217=DIRECTION('center_axis',(0.,-1.,0.));
#6218=DIRECTION('ref_axis',(0.,0.,-1.));
#6219=DIRECTION('center_axis',(0.,0.,1.));
#6220=DIRECTION('ref_axis',(1.,0.,0.));
#6221=DIRECTION('center_axis',(0.,-1.,0.));
#6222=DIRECTION('ref_axis',(0.,0.,-1.));
#6223=DIRECTION('center_axis',(0.,1.,0.));
#6224=DIRECTION('ref_axis',(1.,0.,0.));
#6225=DIRECTION('center_axis',(0.,-1.,0.));
#6226=DIRECTION('ref_axis',(1.,0.,0.));
#6227=DIRECTION('center_axis',(0.,-1.,0.));
#6228=DIRECTION('ref_axis',(0.,0.,-1.));
#6229=DIRECTION('center_axis',(0.,0.,1.));
#6230=DIRECTION('ref_axis',(1.,0.,0.));
#6231=DIRECTION('center_axis',(0.,-1.,0.));
#6232=DIRECTION('ref_axis',(0.,0.,-1.));
#6233=DIRECTION('center_axis',(0.,1.,0.));
#6234=DIRECTION('ref_axis',(1.,0.,0.));
#6235=DIRECTION('center_axis',(0.,1.,0.));
#6236=DIRECTION('ref_axis',(1.,0.,0.));
#6237=DIRECTION('',(0.,1.,0.));
#6238=DIRECTION('center_axis',(0.,-1.,0.));
#6239=DIRECTION('ref_axis',(1.,0.,0.));
#6240=DIRECTION('center_axis',(0.,-1.,0.));
#6241=DIRECTION('ref_axis',(1.,0.,0.));
#6242=DIRECTION('center_axis',(0.,1.,0.));
#6243=DIRECTION('ref_axis',(1.,0.,0.));
#6244=DIRECTION('center_axis',(0.,-1.,0.));
#6245=DIRECTION('ref_axis',(0.,0.,-1.));
#6246=DIRECTION('center_axis',(0.,0.,1.));
#6247=DIRECTION('ref_axis',(1.,0.,0.));
#6248=DIRECTION('center_axis',(0.,-1.,0.));
#6249=DIRECTION('ref_axis',(0.,0.,-1.));
#6250=DIRECTION('center_axis',(0.,-1.,0.));
#6251=DIRECTION('ref_axis',(-1.,0.,0.));
#6252=DIRECTION('center_axis',(0.,1.,0.));
#6253=DIRECTION('ref_axis',(1.,0.,0.));
#6254=DIRECTION('axis',(0.,0.,1.));
#6255=DIRECTION('refdir',(1.,0.,0.));
#6256=DIRECTION('center_axis',(0.,1.,0.));
#6257=DIRECTION('ref_axis',(0.,0.,1.));
#6258=DIRECTION('center_axis',(0.,-1.,0.));
#6259=DIRECTION('ref_axis',(1.,0.,0.));
#6260=DIRECTION('center_axis',(0.,-1.,0.));
#6261=DIRECTION('ref_axis',(1.,0.,0.));
#6262=DIRECTION('center_axis',(0.,-1.,0.));
#6263=DIRECTION('ref_axis',(1.,0.,0.));
#6264=DIRECTION('center_axis',(0.,-1.,0.));
#6265=DIRECTION('ref_axis',(1.,0.,0.));
#6266=DIRECTION('',(0.,1.,0.));
#6267=DIRECTION('center_axis',(0.,-1.,0.));
#6268=DIRECTION('ref_axis',(0.,0.,-1.));
#6269=DIRECTION('center_axis',(0.,-1.,0.));
#6270=DIRECTION('ref_axis',(1.,0.,0.));
#6271=DIRECTION('center_axis',(0.,-1.,0.));
#6272=DIRECTION('ref_axis',(1.,0.,0.));
#6273=DIRECTION('',(0.,1.,0.));
#6274=DIRECTION('center_axis',(0.,1.,0.));
#6275=DIRECTION('ref_axis',(0.,0.,1.));
#6276=DIRECTION('center_axis',(0.,-1.,0.));
#6277=DIRECTION('ref_axis',(1.,0.,0.));
#6278=DIRECTION('center_axis',(0.,-1.,0.));
#6279=DIRECTION('ref_axis',(1.,0.,0.));
#6280=DIRECTION('center_axis',(0.,-1.,0.));
#6281=DIRECTION('ref_axis',(1.,0.,0.));
#6282=DIRECTION('center_axis',(0.,-1.,0.));
#6283=DIRECTION('ref_axis',(1.,0.,0.));
#6284=DIRECTION('',(0.,1.,0.));
#6285=DIRECTION('center_axis',(0.,-1.,0.));
#6286=DIRECTION('ref_axis',(0.,0.,-1.));
#6287=DIRECTION('center_axis',(0.,-1.,0.));
#6288=DIRECTION('ref_axis',(1.,0.,0.));
#6289=DIRECTION('center_axis',(0.,-1.,0.));
#6290=DIRECTION('ref_axis',(1.,0.,0.));
#6291=DIRECTION('',(0.,1.,0.));
#6292=DIRECTION('',(0.,0.,1.));
#6293=DIRECTION('',(1.,0.,0.));
#6294=DIRECTION('',(0.,0.,1.));
#6295=DIRECTION('',(1.,0.,0.));
#6296=DIRECTION('',(0.,0.,1.));
#6297=DIRECTION('',(1.,0.,0.));
#6298=DIRECTION('',(0.,0.,1.));
#6299=DIRECTION('',(1.,0.,0.));
#6300=DIRECTION('',(0.,0.,1.));
#6301=DIRECTION('',(1.,0.,0.));
#6302=DIRECTION('axis',(0.,0.,1.));
#6303=DIRECTION('refdir',(1.,0.,0.));
#6304=DIRECTION('center_axis',(0.,1.,0.));
#6305=DIRECTION('ref_axis',(1.,0.,0.));
#6306=DIRECTION('center_axis',(0.,1.,0.));
#6307=DIRECTION('ref_axis',(1.,0.,0.));
#6308=DIRECTION('center_axis',(0.866025403784439,0.,-0.5));
#6309=DIRECTION('ref_axis',(0.5,0.,0.866025403784439));
#6310=DIRECTION('',(0.5,0.,0.866025403784439));
#6311=DIRECTION('',(0.,-1.,0.));
#6312=DIRECTION('',(0.5,0.,0.866025403784439));
#6313=DIRECTION('',(0.,-1.,0.));
#6314=DIRECTION('center_axis',(1.92296268638356E-16,0.,-1.));
#6315=DIRECTION('ref_axis',(1.,0.,1.92296268638356E-16));
#6316=DIRECTION('',(1.,0.,1.92296268638356E-16));
#6317=DIRECTION('',(0.,-1.,0.));
#6318=DIRECTION('',(1.,0.,1.92296268638356E-16));
#6319=DIRECTION('center_axis',(-0.866025403784439,0.,-0.5));
#6320=DIRECTION('ref_axis',(0.5,0.,-0.866025403784439));
#6321=DIRECTION('',(0.5,0.,-0.866025403784439));
#6322=DIRECTION('',(0.,-1.,0.));
#6323=DIRECTION('',(0.5,0.,-0.866025403784438));
#6324=DIRECTION('center_axis',(-0.866025403784439,0.,0.5));
#6325=DIRECTION('ref_axis',(-0.5,0.,-0.866025403784439));
#6326=DIRECTION('',(-0.5,0.,-0.866025403784439));
#6327=DIRECTION('',(0.,-1.,0.));
#6328=DIRECTION('',(-0.5,0.,-0.866025403784439));
#6329=DIRECTION('center_axis',(-1.92296268638356E-16,0.,1.));
#6330=DIRECTION('ref_axis',(-1.,0.,-1.92296268638356E-16));
#6331=DIRECTION('',(-1.,0.,-1.92296268638356E-16));
#6332=DIRECTION('',(0.,-1.,0.));
#6333=DIRECTION('',(-1.,0.,-1.92296268638356E-16));
#6334=DIRECTION('center_axis',(0.866025403784439,0.,0.5));
#6335=DIRECTION('ref_axis',(-0.5,0.,0.866025403784439));
#6336=DIRECTION('',(-0.5,0.,0.866025403784439));
#6337=DIRECTION('',(-0.5,0.,0.866025403784439));
#6338=DIRECTION('center_axis',(0.,-1.,0.));
#6339=DIRECTION('ref_axis',(0.,0.,-1.));
#6340=DIRECTION('center_axis',(0.,1.,0.));
#6341=DIRECTION('ref_axis',(0.,0.,1.));
#6342=DIRECTION('center_axis',(0.,-1.,0.));
#6343=DIRECTION('ref_axis',(1.,0.,0.));
#6344=DIRECTION('center_axis',(0.,-1.,0.));
#6345=DIRECTION('ref_axis',(1.,0.,0.));
#6346=DIRECTION('center_axis',(0.,-1.,0.));
#6347=DIRECTION('ref_axis',(1.,0.,0.));
#6348=DIRECTION('',(0.707106781186547,0.707106781186548,8.65956056235493E-17));
#6349=DIRECTION('center_axis',(0.,-1.,0.));
#6350=DIRECTION('ref_axis',(1.,0.,0.));
#6351=DIRECTION('',(0.,1.,0.));
#6352=DIRECTION('axis',(0.,0.,1.));
#6353=DIRECTION('refdir',(1.,0.,0.));
#6354=DIRECTION('axis',(0.,0.,1.));
#6355=DIRECTION('refdir',(1.,0.,0.));
#6356=DIRECTION('center_axis',(0.,0.,1.));
#6357=DIRECTION('ref_axis',(1.,0.,0.));
#6358=DIRECTION('center_axis',(0.,0.,1.));
#6359=DIRECTION('ref_axis',(1.,0.,0.));
#6360=DIRECTION('',(0.,0.,1.));
#6361=DIRECTION('center_axis',(0.,0.,1.));
#6362=DIRECTION('ref_axis',(1.,0.,0.));
#6363=DIRECTION('center_axis',(0.,0.,1.));
#6364=DIRECTION('ref_axis',(1.,0.,0.));
#6365=DIRECTION('center_axis',(0.,0.,1.));
#6366=DIRECTION('ref_axis',(1.,0.,0.));
#6367=DIRECTION('center_axis',(0.,0.,1.));
#6368=DIRECTION('ref_axis',(1.,0.,0.));
#6369=DIRECTION('',(0.,0.,1.));
#6370=DIRECTION('center_axis',(0.,0.,1.));
#6371=DIRECTION('ref_axis',(1.,0.,0.));
#6372=DIRECTION('center_axis',(0.,0.,1.));
#6373=DIRECTION('ref_axis',(1.,0.,0.));
#6374=DIRECTION('center_axis',(0.,0.,1.));
#6375=DIRECTION('ref_axis',(1.,0.,0.));
#6376=DIRECTION('center_axis',(0.,0.,1.));
#6377=DIRECTION('ref_axis',(1.,0.,0.));
#6378=DIRECTION('',(0.,0.,1.));
#6379=DIRECTION('center_axis',(0.,0.,1.));
#6380=DIRECTION('ref_axis',(1.,0.,0.));
#6381=DIRECTION('center_axis',(0.,0.,1.));
#6382=DIRECTION('ref_axis',(1.,0.,0.));
#6383=DIRECTION('center_axis',(0.,0.,1.));
#6384=DIRECTION('ref_axis',(1.,0.,0.));
#6385=DIRECTION('center_axis',(0.,0.,1.));
#6386=DIRECTION('ref_axis',(1.,0.,0.));
#6387=DIRECTION('',(0.,0.,1.));
#6388=DIRECTION('center_axis',(0.,0.,1.));
#6389=DIRECTION('ref_axis',(1.,0.,0.));
#6390=DIRECTION('center_axis',(0.,0.,1.));
#6391=DIRECTION('ref_axis',(1.,0.,0.));
#6392=DIRECTION('center_axis',(0.,0.,1.));
#6393=DIRECTION('ref_axis',(1.,0.,0.));
#6394=DIRECTION('center_axis',(0.,0.,1.));
#6395=DIRECTION('ref_axis',(1.,0.,0.));
#6396=DIRECTION('',(0.,0.,1.));
#6397=DIRECTION('center_axis',(0.,0.,1.));
#6398=DIRECTION('ref_axis',(1.,0.,0.));
#6399=DIRECTION('center_axis',(0.,0.,1.));
#6400=DIRECTION('ref_axis',(1.,0.,0.));
#6401=DIRECTION('center_axis',(0.,0.,1.));
#6402=DIRECTION('ref_axis',(1.,0.,0.));
#6403=DIRECTION('center_axis',(0.,0.,1.));
#6404=DIRECTION('ref_axis',(1.,0.,0.));
#6405=DIRECTION('',(0.,0.,1.));
#6406=DIRECTION('center_axis',(0.,0.,1.));
#6407=DIRECTION('ref_axis',(1.,0.,0.));
#6408=DIRECTION('center_axis',(0.,0.,1.));
#6409=DIRECTION('ref_axis',(1.,0.,0.));
#6410=DIRECTION('center_axis',(0.,0.,1.));
#6411=DIRECTION('ref_axis',(1.,0.,0.));
#6412=DIRECTION('center_axis',(0.,0.,1.));
#6413=DIRECTION('ref_axis',(1.,0.,0.));
#6414=DIRECTION('',(0.,0.,1.));
#6415=DIRECTION('center_axis',(0.,0.,1.));
#6416=DIRECTION('ref_axis',(1.,0.,0.));
#6417=DIRECTION('center_axis',(0.,0.,1.));
#6418=DIRECTION('ref_axis',(1.,0.,0.));
#6419=DIRECTION('center_axis',(0.,0.,1.));
#6420=DIRECTION('ref_axis',(1.,0.,0.));
#6421=DIRECTION('center_axis',(0.,0.,1.));
#6422=DIRECTION('ref_axis',(1.,0.,0.));
#6423=DIRECTION('',(0.,0.,1.));
#6424=DIRECTION('center_axis',(0.,0.,1.));
#6425=DIRECTION('ref_axis',(1.,0.,0.));
#6426=DIRECTION('center_axis',(0.,0.,1.));
#6427=DIRECTION('ref_axis',(1.,0.,0.));
#6428=DIRECTION('center_axis',(0.,0.,1.));
#6429=DIRECTION('ref_axis',(1.,0.,0.));
#6430=DIRECTION('center_axis',(0.,0.,1.));
#6431=DIRECTION('ref_axis',(1.,0.,0.));
#6432=DIRECTION('',(0.,0.,1.));
#6433=DIRECTION('center_axis',(0.,0.,1.));
#6434=DIRECTION('ref_axis',(1.,0.,0.));
#6435=DIRECTION('center_axis',(0.,0.,1.));
#6436=DIRECTION('ref_axis',(1.,0.,0.));
#6437=DIRECTION('center_axis',(0.,0.,1.));
#6438=DIRECTION('ref_axis',(1.,0.,0.));
#6439=DIRECTION('center_axis',(0.,0.,1.));
#6440=DIRECTION('ref_axis',(1.,0.,0.));
#6441=DIRECTION('',(0.,0.,1.));
#6442=DIRECTION('center_axis',(0.,0.,1.));
#6443=DIRECTION('ref_axis',(1.,0.,0.));
#6444=DIRECTION('center_axis',(0.,0.,1.));
#6445=DIRECTION('ref_axis',(1.,0.,0.));
#6446=DIRECTION('center_axis',(0.,0.,1.));
#6447=DIRECTION('ref_axis',(1.,0.,0.));
#6448=DIRECTION('center_axis',(0.,0.,1.));
#6449=DIRECTION('ref_axis',(1.,0.,0.));
#6450=DIRECTION('',(0.,0.,1.));
#6451=DIRECTION('center_axis',(0.,0.,1.));
#6452=DIRECTION('ref_axis',(1.,0.,0.));
#6453=DIRECTION('center_axis',(0.,0.,1.));
#6454=DIRECTION('ref_axis',(1.,0.,0.));
#6455=DIRECTION('center_axis',(0.,0.,1.));
#6456=DIRECTION('ref_axis',(1.,0.,0.));
#6457=DIRECTION('center_axis',(0.,0.,1.));
#6458=DIRECTION('ref_axis',(1.,0.,0.));
#6459=DIRECTION('',(0.,0.,1.));
#6460=DIRECTION('center_axis',(0.,0.,1.));
#6461=DIRECTION('ref_axis',(1.,0.,0.));
#6462=DIRECTION('center_axis',(0.,0.,1.));
#6463=DIRECTION('ref_axis',(1.,0.,0.));
#6464=DIRECTION('center_axis',(0.,0.,1.));
#6465=DIRECTION('ref_axis',(1.,0.,0.));
#6466=DIRECTION('center_axis',(0.,0.,1.));
#6467=DIRECTION('ref_axis',(1.,0.,0.));
#6468=DIRECTION('',(0.,0.,1.));
#6469=DIRECTION('center_axis',(0.,0.,1.));
#6470=DIRECTION('ref_axis',(1.,0.,0.));
#6471=DIRECTION('center_axis',(0.,0.,1.));
#6472=DIRECTION('ref_axis',(1.,0.,0.));
#6473=DIRECTION('center_axis',(0.,0.,1.));
#6474=DIRECTION('ref_axis',(1.,0.,0.));
#6475=DIRECTION('center_axis',(0.,0.,1.));
#6476=DIRECTION('ref_axis',(1.,0.,0.));
#6477=DIRECTION('',(0.,0.,1.));
#6478=DIRECTION('center_axis',(0.,0.,1.));
#6479=DIRECTION('ref_axis',(1.,0.,0.));
#6480=DIRECTION('center_axis',(0.,0.,1.));
#6481=DIRECTION('ref_axis',(1.,0.,0.));
#6482=DIRECTION('center_axis',(0.,0.,1.));
#6483=DIRECTION('ref_axis',(1.,0.,0.));
#6484=DIRECTION('center_axis',(0.,0.,1.));
#6485=DIRECTION('ref_axis',(1.,0.,0.));
#6486=DIRECTION('',(0.,0.,1.));
#6487=DIRECTION('center_axis',(0.,0.,1.));
#6488=DIRECTION('ref_axis',(1.,0.,0.));
#6489=DIRECTION('center_axis',(0.,0.,1.));
#6490=DIRECTION('ref_axis',(1.,0.,0.));
#6491=DIRECTION('center_axis',(0.,0.,1.));
#6492=DIRECTION('ref_axis',(1.,0.,0.));
#6493=DIRECTION('center_axis',(0.,0.,1.));
#6494=DIRECTION('ref_axis',(1.,0.,0.));
#6495=DIRECTION('',(0.,0.,1.));
#6496=DIRECTION('center_axis',(0.,0.,1.));
#6497=DIRECTION('ref_axis',(1.,0.,0.));
#6498=DIRECTION('center_axis',(0.,0.,1.));
#6499=DIRECTION('ref_axis',(1.,0.,0.));
#6500=DIRECTION('center_axis',(0.,0.,1.));
#6501=DIRECTION('ref_axis',(1.,0.,0.));
#6502=DIRECTION('center_axis',(0.,0.,1.));
#6503=DIRECTION('ref_axis',(1.,0.,0.));
#6504=DIRECTION('',(0.,0.,1.));
#6505=DIRECTION('center_axis',(0.,0.,1.));
#6506=DIRECTION('ref_axis',(1.,0.,0.));
#6507=DIRECTION('center_axis',(0.,0.,1.));
#6508=DIRECTION('ref_axis',(1.,0.,0.));
#6509=DIRECTION('center_axis',(0.,0.,1.));
#6510=DIRECTION('ref_axis',(1.,0.,0.));
#6511=DIRECTION('center_axis',(0.,0.,1.));
#6512=DIRECTION('ref_axis',(1.,0.,0.));
#6513=DIRECTION('',(0.,0.,1.));
#6514=DIRECTION('center_axis',(0.,0.,1.));
#6515=DIRECTION('ref_axis',(1.,0.,0.));
#6516=DIRECTION('center_axis',(0.,0.,1.));
#6517=DIRECTION('ref_axis',(1.,0.,0.));
#6518=DIRECTION('center_axis',(0.,0.,1.));
#6519=DIRECTION('ref_axis',(1.,0.,0.));
#6520=DIRECTION('center_axis',(0.,0.,1.));
#6521=DIRECTION('ref_axis',(1.,0.,0.));
#6522=DIRECTION('',(0.,0.,1.));
#6523=DIRECTION('center_axis',(0.,0.,1.));
#6524=DIRECTION('ref_axis',(1.,0.,0.));
#6525=DIRECTION('center_axis',(0.,0.,1.));
#6526=DIRECTION('ref_axis',(1.,0.,0.));
#6527=DIRECTION('center_axis',(0.,0.,1.));
#6528=DIRECTION('ref_axis',(1.,0.,0.));
#6529=DIRECTION('center_axis',(0.,0.,1.));
#6530=DIRECTION('ref_axis',(1.,0.,0.));
#6531=DIRECTION('',(0.,0.,1.));
#6532=DIRECTION('center_axis',(0.,0.,1.));
#6533=DIRECTION('ref_axis',(1.,0.,0.));
#6534=DIRECTION('center_axis',(0.,0.,1.));
#6535=DIRECTION('ref_axis',(1.,0.,0.));
#6536=DIRECTION('center_axis',(0.,0.,1.));
#6537=DIRECTION('ref_axis',(1.,0.,0.));
#6538=DIRECTION('center_axis',(0.,0.,1.));
#6539=DIRECTION('ref_axis',(1.,0.,0.));
#6540=DIRECTION('',(0.,0.,1.));
#6541=DIRECTION('center_axis',(0.,0.,-1.));
#6542=DIRECTION('ref_axis',(1.,0.,0.));
#6543=DIRECTION('center_axis',(0.,0.,1.));
#6544=DIRECTION('ref_axis',(1.,0.,0.));
#6545=DIRECTION('center_axis',(0.,0.,1.));
#6546=DIRECTION('ref_axis',(1.,0.,0.));
#6547=DIRECTION('',(0.,0.,1.));
#6548=DIRECTION('center_axis',(0.,0.,-1.));
#6549=DIRECTION('ref_axis',(1.,0.,0.));
#6550=DIRECTION('center_axis',(0.,0.,1.));
#6551=DIRECTION('ref_axis',(1.,0.,0.));
#6552=DIRECTION('center_axis',(0.,0.,1.));
#6553=DIRECTION('ref_axis',(1.,0.,0.));
#6554=DIRECTION('',(0.,0.,1.));
#6555=DIRECTION('center_axis',(0.,0.,-1.));
#6556=DIRECTION('ref_axis',(1.,0.,0.));
#6557=DIRECTION('center_axis',(0.,0.,1.));
#6558=DIRECTION('ref_axis',(1.,0.,0.));
#6559=DIRECTION('center_axis',(0.,0.,1.));
#6560=DIRECTION('ref_axis',(1.,0.,0.));
#6561=DIRECTION('',(0.,0.,1.));
#6562=DIRECTION('center_axis',(0.,0.,-1.));
#6563=DIRECTION('ref_axis',(1.,0.,0.));
#6564=DIRECTION('center_axis',(0.,0.,1.));
#6565=DIRECTION('ref_axis',(1.,0.,0.));
#6566=DIRECTION('center_axis',(0.,0.,1.));
#6567=DIRECTION('ref_axis',(1.,0.,0.));
#6568=DIRECTION('',(0.,0.,1.));
#6569=DIRECTION('center_axis',(0.,0.,-1.));
#6570=DIRECTION('ref_axis',(1.,0.,0.));
#6571=DIRECTION('center_axis',(0.,0.,1.));
#6572=DIRECTION('ref_axis',(1.,0.,0.));
#6573=DIRECTION('center_axis',(0.,0.,1.));
#6574=DIRECTION('ref_axis',(1.,0.,0.));
#6575=DIRECTION('',(0.,0.,1.));
#6576=DIRECTION('center_axis',(0.,0.,-1.));
#6577=DIRECTION('ref_axis',(1.,0.,0.));
#6578=DIRECTION('center_axis',(0.,0.,1.));
#6579=DIRECTION('ref_axis',(1.,0.,0.));
#6580=DIRECTION('center_axis',(0.,0.,1.));
#6581=DIRECTION('ref_axis',(1.,0.,0.));
#6582=DIRECTION('',(0.,0.,1.));
#6583=DIRECTION('center_axis',(0.,0.,-1.));
#6584=DIRECTION('ref_axis',(1.,0.,0.));
#6585=DIRECTION('center_axis',(0.,0.,1.));
#6586=DIRECTION('ref_axis',(1.,0.,0.));
#6587=DIRECTION('center_axis',(0.,0.,1.));
#6588=DIRECTION('ref_axis',(1.,0.,0.));
#6589=DIRECTION('',(0.,0.,1.));
#6590=DIRECTION('center_axis',(0.,0.,-1.));
#6591=DIRECTION('ref_axis',(1.,0.,0.));
#6592=DIRECTION('center_axis',(0.,0.,1.));
#6593=DIRECTION('ref_axis',(1.,0.,0.));
#6594=DIRECTION('center_axis',(0.,0.,-1.));
#6595=DIRECTION('ref_axis',(1.,0.,0.));
#6596=DIRECTION('center_axis',(0.,0.,-1.));
#6597=DIRECTION('ref_axis',(1.,0.,0.));
#6598=DIRECTION('center_axis',(0.,0.,1.));
#6599=DIRECTION('ref_axis',(1.,0.,0.));
#6600=DIRECTION('',(0.,0.,-1.));
#6601=DIRECTION('center_axis',(0.,0.,-1.));
#6602=DIRECTION('ref_axis',(1.,0.,0.));
#6603=DIRECTION('center_axis',(0.,0.,1.));
#6604=DIRECTION('ref_axis',(1.,0.,0.));
#6605=DIRECTION('center_axis',(0.,0.,1.));
#6606=DIRECTION('ref_axis',(1.,0.,0.));
#6607=DIRECTION('center_axis',(0.,0.,1.));
#6608=DIRECTION('ref_axis',(1.,0.,0.));
#6609=DIRECTION('center_axis',(0.,0.,1.));
#6610=DIRECTION('ref_axis',(1.,0.,0.));
#6611=DIRECTION('center_axis',(0.,0.,1.));
#6612=DIRECTION('ref_axis',(1.,0.,0.));
#6613=DIRECTION('center_axis',(0.,0.,1.));
#6614=DIRECTION('ref_axis',(1.,0.,0.));
#6615=DIRECTION('center_axis',(0.,0.,-1.));
#6616=DIRECTION('ref_axis',(1.,0.,0.));
#6617=DIRECTION('',(0.,0.,-1.));
#6618=DIRECTION('center_axis',(0.,0.,1.));
#6619=DIRECTION('ref_axis',(1.,0.,0.));
#6620=DIRECTION('center_axis',(0.,0.,1.));
#6621=DIRECTION('ref_axis',(1.,0.,0.));
#6622=DIRECTION('',(0.,0.,-1.));
#6623=DIRECTION('center_axis',(0.,0.,1.));
#6624=DIRECTION('ref_axis',(1.,0.,0.));
#6625=DIRECTION('center_axis',(0.,0.,1.));
#6626=DIRECTION('ref_axis',(1.,0.,0.));
#6627=DIRECTION('',(0.,0.,-1.));
#6628=DIRECTION('center_axis',(0.,0.,-1.));
#6629=DIRECTION('ref_axis',(1.,0.,0.));
#6630=DIRECTION('center_axis',(0.,0.,1.));
#6631=DIRECTION('ref_axis',(1.,0.,0.));
#6632=DIRECTION('',(0.,0.,-1.));
#6633=DIRECTION('center_axis',(0.,0.,1.));
#6634=DIRECTION('ref_axis',(1.,0.,0.));
#6635=DIRECTION('center_axis',(0.,0.,1.));
#6636=DIRECTION('ref_axis',(1.,0.,0.));
#6637=DIRECTION('axis',(0.,0.,1.));
#6638=DIRECTION('refdir',(1.,0.,0.));
#6639=DIRECTION('center_axis',(0.,0.,1.));
#6640=DIRECTION('ref_axis',(1.,0.,0.));
#6641=DIRECTION('center_axis',(0.,0.,-1.));
#6642=DIRECTION('ref_axis',(1.,0.,0.));
#6643=DIRECTION('',(0.,0.,-1.));
#6644=DIRECTION('center_axis',(0.,0.,-1.));
#6645=DIRECTION('ref_axis',(1.,0.,0.));
#6646=DIRECTION('center_axis',(0.,0.,1.));
#6647=DIRECTION('ref_axis',(1.,0.,0.));
#6648=DIRECTION('center_axis',(0.,0.,1.));
#6649=DIRECTION('ref_axis',(1.,0.,0.));
#6650=DIRECTION('',(0.,0.,-1.));
#6651=DIRECTION('center_axis',(0.,0.,1.));
#6652=DIRECTION('ref_axis',(1.,0.,0.));
#6653=DIRECTION('center_axis',(0.,0.,1.));
#6654=DIRECTION('ref_axis',(1.,0.,0.));
#6655=DIRECTION('center_axis',(0.,0.,1.));
#6656=DIRECTION('ref_axis',(1.,0.,0.));
#6657=DIRECTION('axis',(0.,0.,1.));
#6658=DIRECTION('refdir',(1.,0.,0.));
#6659=DIRECTION('center_axis',(0.,0.,1.));
#6660=DIRECTION('ref_axis',(1.,0.,0.));
#6661=DIRECTION('center_axis',(0.,0.,1.));
#6662=DIRECTION('ref_axis',(1.,0.,0.));
#6663=DIRECTION('',(0.,0.,1.));
#6664=DIRECTION('center_axis',(0.,0.,-1.));
#6665=DIRECTION('ref_axis',(1.,0.,0.));
#6666=DIRECTION('center_axis',(0.,0.,1.));
#6667=DIRECTION('ref_axis',(1.,0.,0.));
#6668=DIRECTION('center_axis',(0.,0.,1.));
#6669=DIRECTION('ref_axis',(1.,0.,0.));
#6670=DIRECTION('',(0.,0.,1.));
#6671=DIRECTION('center_axis',(0.,0.,-1.));
#6672=DIRECTION('ref_axis',(1.,0.,0.));
#6673=DIRECTION('center_axis',(0.,0.,1.));
#6674=DIRECTION('ref_axis',(1.,0.,0.));
#6675=DIRECTION('center_axis',(0.,0.,1.));
#6676=DIRECTION('ref_axis',(1.,0.,0.));
#6677=DIRECTION('',(0.,0.,1.));
#6678=DIRECTION('center_axis',(0.,0.,-1.));
#6679=DIRECTION('ref_axis',(1.,0.,0.));
#6680=DIRECTION('center_axis',(0.,0.,1.));
#6681=DIRECTION('ref_axis',(1.,0.,0.));
#6682=DIRECTION('center_axis',(0.,0.,1.));
#6683=DIRECTION('ref_axis',(1.,0.,0.));
#6684=DIRECTION('',(0.,0.,1.));
#6685=DIRECTION('center_axis',(0.,0.,-1.));
#6686=DIRECTION('ref_axis',(1.,0.,0.));
#6687=DIRECTION('center_axis',(0.,0.,1.));
#6688=DIRECTION('ref_axis',(1.,0.,0.));
#6689=DIRECTION('center_axis',(0.,0.,1.));
#6690=DIRECTION('ref_axis',(1.,0.,0.));
#6691=DIRECTION('',(0.,0.,-1.));
#6692=DIRECTION('center_axis',(0.,0.,-1.));
#6693=DIRECTION('ref_axis',(1.,0.,0.));
#6694=DIRECTION('center_axis',(0.,0.,1.));
#6695=DIRECTION('ref_axis',(1.,0.,0.));
#6696=DIRECTION('center_axis',(0.,0.,-1.));
#6697=DIRECTION('ref_axis',(1.,0.,0.));
#6698=DIRECTION('center_axis',(0.,0.,1.));
#6699=DIRECTION('ref_axis',(1.,0.,0.));
#6700=DIRECTION('',(0.,0.,-1.));
#6701=DIRECTION('center_axis',(0.,0.,-1.));
#6702=DIRECTION('ref_axis',(1.,0.,0.));
#6703=DIRECTION('center_axis',(0.,0.,1.));
#6704=DIRECTION('ref_axis',(1.,0.,0.));
#6705=DIRECTION('center_axis',(0.,0.,1.));
#6706=DIRECTION('ref_axis',(1.,0.,0.));
#6707=DIRECTION('',(0.,0.,-1.));
#6708=DIRECTION('center_axis',(0.,0.,1.));
#6709=DIRECTION('ref_axis',(1.,0.,0.));
#6710=DIRECTION('center_axis',(0.,0.,1.));
#6711=DIRECTION('ref_axis',(1.,0.,0.));
#6712=DIRECTION('center_axis',(0.,0.,1.));
#6713=DIRECTION('ref_axis',(1.,0.,0.));
#6714=DIRECTION('axis',(0.,0.,1.));
#6715=DIRECTION('refdir',(1.,0.,0.));
#6716=DIRECTION('center_axis',(0.,0.,1.));
#6717=DIRECTION('ref_axis',(1.,0.,0.));
#6718=DIRECTION('center_axis',(0.,0.,1.));
#6719=DIRECTION('ref_axis',(1.,0.,0.));
#6720=DIRECTION('',(0.,0.,1.));
#6721=DIRECTION('center_axis',(0.,0.,-1.));
#6722=DIRECTION('ref_axis',(1.,0.,0.));
#6723=DIRECTION('center_axis',(0.,0.,1.));
#6724=DIRECTION('ref_axis',(1.,0.,0.));
#6725=DIRECTION('center_axis',(0.,0.,1.));
#6726=DIRECTION('ref_axis',(1.,0.,0.));
#6727=DIRECTION('',(0.,0.,1.));
#6728=DIRECTION('center_axis',(0.,0.,-1.));
#6729=DIRECTION('ref_axis',(1.,0.,0.));
#6730=DIRECTION('center_axis',(0.,0.,1.));
#6731=DIRECTION('ref_axis',(1.,0.,0.));
#6732=DIRECTION('center_axis',(0.,0.,1.));
#6733=DIRECTION('ref_axis',(1.,0.,0.));
#6734=DIRECTION('',(0.,0.,1.));
#6735=DIRECTION('center_axis',(0.,0.,-1.));
#6736=DIRECTION('ref_axis',(1.,0.,0.));
#6737=DIRECTION('center_axis',(0.,0.,1.));
#6738=DIRECTION('ref_axis',(1.,0.,0.));
#6739=DIRECTION('center_axis',(0.,0.,1.));
#6740=DIRECTION('ref_axis',(1.,0.,0.));
#6741=DIRECTION('',(0.,0.,1.));
#6742=DIRECTION('center_axis',(0.,0.,-1.));
#6743=DIRECTION('ref_axis',(1.,0.,0.));
#6744=DIRECTION('center_axis',(0.,0.,1.));
#6745=DIRECTION('ref_axis',(1.,0.,0.));
#6746=DIRECTION('center_axis',(0.,0.,1.));
#6747=DIRECTION('ref_axis',(1.,0.,0.));
#6748=DIRECTION('',(0.,0.,1.));
#6749=DIRECTION('center_axis',(0.,0.,-1.));
#6750=DIRECTION('ref_axis',(1.,0.,0.));
#6751=DIRECTION('center_axis',(0.,0.,1.));
#6752=DIRECTION('ref_axis',(1.,0.,0.));
#6753=DIRECTION('center_axis',(0.,0.,1.));
#6754=DIRECTION('ref_axis',(1.,0.,0.));
#6755=DIRECTION('',(0.,0.,1.));
#6756=DIRECTION('center_axis',(0.,0.,-1.));
#6757=DIRECTION('ref_axis',(1.,0.,0.));
#6758=DIRECTION('center_axis',(0.,0.,1.));
#6759=DIRECTION('ref_axis',(1.,0.,0.));
#6760=DIRECTION('center_axis',(0.,0.,1.));
#6761=DIRECTION('ref_axis',(1.,0.,0.));
#6762=DIRECTION('',(0.,0.,1.));
#6763=DIRECTION('center_axis',(0.,0.,-1.));
#6764=DIRECTION('ref_axis',(1.,0.,0.));
#6765=DIRECTION('center_axis',(0.,0.,1.));
#6766=DIRECTION('ref_axis',(1.,0.,0.));
#6767=DIRECTION('center_axis',(0.,0.,1.));
#6768=DIRECTION('ref_axis',(1.,0.,0.));
#6769=DIRECTION('',(0.,0.,1.));
#6770=DIRECTION('center_axis',(0.,0.,-1.));
#6771=DIRECTION('ref_axis',(1.,0.,0.));
#6772=DIRECTION('center_axis',(0.,0.,1.));
#6773=DIRECTION('ref_axis',(1.,0.,0.));
#6774=DIRECTION('center_axis',(0.,0.,1.));
#6775=DIRECTION('ref_axis',(1.,0.,0.));
#6776=DIRECTION('',(0.,0.,1.));
#6777=DIRECTION('center_axis',(0.,0.,-1.));
#6778=DIRECTION('ref_axis',(1.,0.,0.));
#6779=DIRECTION('center_axis',(0.,0.,1.));
#6780=DIRECTION('ref_axis',(1.,0.,0.));
#6781=DIRECTION('center_axis',(0.,0.,1.));
#6782=DIRECTION('ref_axis',(1.,0.,0.));
#6783=DIRECTION('',(0.,0.,1.));
#6784=DIRECTION('center_axis',(0.,0.,-1.));
#6785=DIRECTION('ref_axis',(1.,0.,0.));
#6786=DIRECTION('center_axis',(0.,0.,1.));
#6787=DIRECTION('ref_axis',(1.,0.,0.));
#6788=DIRECTION('center_axis',(0.,0.,1.));
#6789=DIRECTION('ref_axis',(1.,0.,0.));
#6790=DIRECTION('',(0.,0.,1.));
#6791=DIRECTION('center_axis',(0.,0.,-1.));
#6792=DIRECTION('ref_axis',(1.,0.,0.));
#6793=DIRECTION('center_axis',(0.,0.,1.));
#6794=DIRECTION('ref_axis',(1.,0.,0.));
#6795=DIRECTION('center_axis',(0.,0.,1.));
#6796=DIRECTION('ref_axis',(1.,0.,0.));
#6797=DIRECTION('',(0.,0.,1.));
#6798=DIRECTION('center_axis',(0.,0.,-1.));
#6799=DIRECTION('ref_axis',(1.,0.,0.));
#6800=DIRECTION('center_axis',(0.,0.,1.));
#6801=DIRECTION('ref_axis',(1.,0.,0.));
#6802=DIRECTION('center_axis',(0.,0.,1.));
#6803=DIRECTION('ref_axis',(1.,0.,0.));
#6804=DIRECTION('',(0.,0.,1.));
#6805=DIRECTION('center_axis',(0.,0.,-1.));
#6806=DIRECTION('ref_axis',(1.,0.,0.));
#6807=DIRECTION('center_axis',(0.,0.,1.));
#6808=DIRECTION('ref_axis',(1.,0.,0.));
#6809=DIRECTION('center_axis',(0.,0.,1.));
#6810=DIRECTION('ref_axis',(1.,0.,0.));
#6811=DIRECTION('',(0.,0.,1.));
#6812=DIRECTION('center_axis',(0.,0.,-1.));
#6813=DIRECTION('ref_axis',(1.,0.,0.));
#6814=DIRECTION('center_axis',(0.,0.,1.));
#6815=DIRECTION('ref_axis',(1.,0.,0.));
#6816=DIRECTION('center_axis',(0.,0.,1.));
#6817=DIRECTION('ref_axis',(1.,0.,0.));
#6818=DIRECTION('',(0.,0.,1.));
#6819=DIRECTION('center_axis',(0.,0.,-1.));
#6820=DIRECTION('ref_axis',(1.,0.,0.));
#6821=DIRECTION('center_axis',(0.,0.,1.));
#6822=DIRECTION('ref_axis',(1.,0.,0.));
#6823=DIRECTION('center_axis',(0.,0.,1.));
#6824=DIRECTION('ref_axis',(1.,0.,0.));
#6825=DIRECTION('',(0.,0.,1.));
#6826=DIRECTION('center_axis',(0.,0.,-1.));
#6827=DIRECTION('ref_axis',(1.,0.,0.));
#6828=DIRECTION('center_axis',(0.,0.,1.));
#6829=DIRECTION('ref_axis',(1.,0.,0.));
#6830=DIRECTION('center_axis',(0.,0.,-1.));
#6831=DIRECTION('ref_axis',(1.,0.,0.));
#6832=DIRECTION('',(0.,0.,-1.));
#6833=DIRECTION('center_axis',(0.,0.,-1.));
#6834=DIRECTION('ref_axis',(1.,0.,0.));
#6835=DIRECTION('center_axis',(0.,0.,1.));
#6836=DIRECTION('ref_axis',(1.,0.,0.));
#6837=DIRECTION('center_axis',(0.,0.,1.));
#6838=DIRECTION('ref_axis',(1.,0.,0.));
#6839=DIRECTION('',(0.,0.,-1.));
#6840=DIRECTION('center_axis',(0.,0.,1.));
#6841=DIRECTION('ref_axis',(1.,0.,0.));
#6842=DIRECTION('center_axis',(0.,0.,1.));
#6843=DIRECTION('ref_axis',(1.,0.,0.));
#6844=DIRECTION('center_axis',(0.,0.,1.));
#6845=DIRECTION('ref_axis',(1.,0.,0.));
#6846=DIRECTION('axis',(0.,0.,1.));
#6847=DIRECTION('refdir',(1.,0.,0.));
#6848=DIRECTION('center_axis',(0.,1.,0.));
#6849=DIRECTION('ref_axis',(0.,0.,1.));
#6850=DIRECTION('center_axis',(0.,-1.,0.));
#6851=DIRECTION('ref_axis',(1.,0.,0.));
#6852=DIRECTION('center_axis',(0.,-1.,0.));
#6853=DIRECTION('ref_axis',(1.,0.,0.));
#6854=DIRECTION('center_axis',(0.,-1.,0.));
#6855=DIRECTION('ref_axis',(1.,0.,0.));
#6856=DIRECTION('',(0.707106781186547,0.707106781186548,8.65956056235493E-17));
#6857=DIRECTION('center_axis',(0.,-1.,0.));
#6858=DIRECTION('ref_axis',(1.,0.,0.));
#6859=DIRECTION('center_axis',(0.,-1.,0.));
#6860=DIRECTION('ref_axis',(1.,0.,0.));
#6861=DIRECTION('',(0.,1.,0.));
#6862=DIRECTION('center_axis',(0.,1.,0.));
#6863=DIRECTION('ref_axis',(1.,0.,0.));
#6864=DIRECTION('center_axis',(0.,-1.,0.));
#6865=DIRECTION('ref_axis',(1.,0.,0.));
#6866=DIRECTION('',(-0.707106781186547,0.707106781186548,-8.65956056235493E-17));
#6867=DIRECTION('center_axis',(0.,-1.,0.));
#6868=DIRECTION('ref_axis',(0.,0.,-1.));
#6869=DIRECTION('center_axis',(0.,-1.,0.));
#6870=DIRECTION('ref_axis',(1.,0.,0.));
#6871=DIRECTION('center_axis',(0.,1.,0.));
#6872=DIRECTION('ref_axis',(1.,0.,0.));
#6873=DIRECTION('center_axis',(0.,1.,0.));
#6874=DIRECTION('ref_axis',(1.,0.,0.));
#6875=DIRECTION('',(-0.447213595499958,0.894427190999916,-5.47678698264203E-17));
#6876=DIRECTION('center_axis',(0.,-1.,0.));
#6877=DIRECTION('ref_axis',(1.,0.,0.));
#6878=DIRECTION('center_axis',(0.,1.,0.));
#6879=DIRECTION('ref_axis',(1.,0.,0.));
#6880=DIRECTION('',(0.,1.,0.));
#6881=DIRECTION('center_axis',(0.,1.,0.));
#6882=DIRECTION('ref_axis',(1.,0.,0.));
#6883=DIRECTION('center_axis',(0.,-1.,0.));
#6884=DIRECTION('ref_axis',(1.,0.,0.));
#6885=DIRECTION('',(-0.707106781186547,0.707106781186548,-8.65956056235493E-17));
#6886=DIRECTION('center_axis',(0.,-1.,0.));
#6887=DIRECTION('ref_axis',(0.,0.,-1.));
#6888=DIRECTION('center_axis',(0.866025403784439,0.,-0.5));
#6889=DIRECTION('ref_axis',(0.5,0.,0.866025403784439));
#6890=DIRECTION('',(-0.5,0.,-0.866025403784439));
#6891=DIRECTION('',(0.,-1.,0.));
#6892=DIRECTION('',(0.5,0.,0.866025403784439));
#6893=DIRECTION('',(0.,-1.,0.));
#6894=DIRECTION('center_axis',(1.60246890531964E-16,0.,-1.));
#6895=DIRECTION('ref_axis',(1.,0.,1.60246890531964E-16));
#6896=DIRECTION('',(-1.,0.,-1.60246890531964E-16));
#6897=DIRECTION('',(0.,-1.,0.));
#6898=DIRECTION('',(1.,0.,1.60246890531964E-16));
#6899=DIRECTION('center_axis',(-0.866025403784439,0.,-0.5));
#6900=DIRECTION('ref_axis',(0.5,0.,-0.866025403784439));
#6901=DIRECTION('',(-0.5,0.,0.866025403784439));
#6902=DIRECTION('',(0.,-1.,0.));
#6903=DIRECTION('',(0.5,0.,-0.866025403784439));
#6904=DIRECTION('center_axis',(-0.866025403784439,0.,0.5));
#6905=DIRECTION('ref_axis',(-0.5,0.,-0.866025403784439));
#6906=DIRECTION('',(0.5,0.,0.866025403784439));
#6907=DIRECTION('',(0.,-1.,0.));
#6908=DIRECTION('',(-0.5,0.,-0.866025403784439));
#6909=DIRECTION('center_axis',(-1.60246890531964E-16,0.,1.));
#6910=DIRECTION('ref_axis',(-1.,0.,-1.60246890531964E-16));
#6911=DIRECTION('',(1.,0.,1.60246890531964E-16));
#6912=DIRECTION('',(0.,-1.,0.));
#6913=DIRECTION('',(-1.,0.,-1.60246890531964E-16));
#6914=DIRECTION('center_axis',(0.866025403784439,0.,0.5));
#6915=DIRECTION('ref_axis',(-0.5,0.,0.866025403784439));
#6916=DIRECTION('',(0.5,0.,-0.866025403784439));
#6917=DIRECTION('',(-0.5,0.,0.866025403784439));
#6918=DIRECTION('center_axis',(0.,1.,0.));
#6919=DIRECTION('ref_axis',(1.,0.,0.));
#6920=DIRECTION('center_axis',(0.,-1.,0.));
#6921=DIRECTION('ref_axis',(0.,0.,-1.));
#6922=DIRECTION('',(0.,0.,1.));
#6923=DIRECTION('',(1.,0.,0.));
#6924=DIRECTION('',(0.,0.,1.));
#6925=DIRECTION('',(1.,0.,0.));
#6926=DIRECTION('',(0.,0.,1.));
#6927=DIRECTION('',(1.,0.,0.));
#6928=DIRECTION('',(0.,0.,1.));
#6929=DIRECTION('',(1.,0.,0.));
#6930=DIRECTION('',(0.,0.,1.));
#6931=DIRECTION('',(1.,0.,0.));
#6932=DIRECTION('',(0.,0.,1.));
#6933=DIRECTION('',(1.,0.,0.));
#6934=DIRECTION('',(0.,0.,1.));
#6935=DIRECTION('',(1.,0.,0.));
#6936=DIRECTION('',(0.,0.,1.));
#6937=DIRECTION('',(1.,0.,0.));
#6938=DIRECTION('',(0.,0.,1.));
#6939=DIRECTION('',(1.,0.,0.));
#6940=DIRECTION('',(0.,0.,1.));
#6941=DIRECTION('',(1.,0.,0.));
#6942=DIRECTION('',(0.,0.,1.));
#6943=DIRECTION('',(1.,0.,0.));
#6944=DIRECTION('',(0.,-1.,2.22044604925031E-16));
#6945=DIRECTION('',(1.,0.,0.));
#6946=DIRECTION('',(0.,-1.,2.22044604925031E-16));
#6947=DIRECTION('',(1.,0.,0.));
#6948=DIRECTION('',(0.,-1.,2.22044604925031E-16));
#6949=DIRECTION('',(1.,0.,0.));
#6950=DIRECTION('',(0.,-1.,2.22044604925031E-16));
#6951=DIRECTION('',(1.,0.,0.));
#6952=DIRECTION('',(0.,-1.,2.22044604925031E-16));
#6953=DIRECTION('',(1.,0.,0.));
#6954=DIRECTION('',(0.,-1.,2.22044604925031E-16));
#6955=DIRECTION('',(1.,0.,0.));
#6956=DIRECTION('',(0.,-1.,2.22044604925031E-16));
#6957=DIRECTION('',(1.,0.,0.));
#6958=DIRECTION('',(0.,-1.,2.22044604925031E-16));
#6959=DIRECTION('',(1.,0.,0.));
#6960=DIRECTION('',(0.,-1.,2.22044604925031E-16));
#6961=DIRECTION('',(1.,0.,0.));
#6962=DIRECTION('',(0.,0.,1.));
#6963=DIRECTION('',(2.22044604925031E-16,-1.,0.));
#6964=DIRECTION('',(0.,-1.,2.22044604925031E-16));
#6965=DIRECTION('',(1.,0.,0.));
#6966=DIRECTION('',(0.,-1.,2.22044604925031E-16));
#6967=DIRECTION('',(1.,0.,0.));
#6968=DIRECTION('',(0.,0.,1.));
#6969=DIRECTION('',(1.,0.,0.));
#6970=DIRECTION('',(0.,0.,1.));
#6971=DIRECTION('',(1.,0.,0.));
#6972=DIRECTION('',(0.,0.,1.));
#6973=DIRECTION('',(1.,0.,0.));
#6974=DIRECTION('',(0.,0.,1.));
#6975=DIRECTION('',(1.,0.,0.));
#6976=DIRECTION('',(0.,1.,2.22044604925031E-16));
#6977=DIRECTION('',(1.,0.,0.));
#6978=DIRECTION('',(0.,1.,2.22044604925031E-16));
#6979=DIRECTION('',(1.,0.,0.));
#6980=DIRECTION('',(0.,1.,2.22044604925031E-16));
#6981=DIRECTION('',(1.,0.,0.));
#6982=DIRECTION('',(0.,1.,2.22044604925031E-16));
#6983=DIRECTION('',(1.,0.,0.));
#6984=DIRECTION('',(0.,1.,2.22044604925031E-16));
#6985=DIRECTION('',(1.,0.,0.));
#6986=DIRECTION('',(0.,1.,2.22044604925031E-16));
#6987=DIRECTION('',(1.,0.,0.));
#6988=DIRECTION('',(0.,1.,2.22044604925031E-16));
#6989=DIRECTION('',(1.,0.,0.));
#6990=DIRECTION('',(0.,1.,2.22044604925031E-16));
#6991=DIRECTION('',(1.,0.,0.));
#6992=DIRECTION('axis',(0.,0.,1.));
#6993=DIRECTION('refdir',(1.,0.,0.));
#6994=DIRECTION('axis',(0.,0.,1.));
#6995=DIRECTION('refdir',(1.,0.,0.));
#6996=DIRECTION('center_axis',(0.,0.,1.));
#6997=DIRECTION('ref_axis',(1.,0.,0.));
#6998=DIRECTION('center_axis',(0.,0.,1.));
#6999=DIRECTION('ref_axis',(1.,0.,0.));
#7000=DIRECTION('center_axis',(0.,0.,1.));
#7001=DIRECTION('ref_axis',(1.,0.,0.));
#7002=DIRECTION('center_axis',(0.,0.,1.));
#7003=DIRECTION('ref_axis',(1.,0.,0.));
#7004=DIRECTION('center_axis',(0.,0.,1.));
#7005=DIRECTION('ref_axis',(1.,0.,0.));
#7006=DIRECTION('center_axis',(0.,0.,1.));
#7007=DIRECTION('ref_axis',(1.,0.,0.));
#7008=DIRECTION('center_axis',(0.,0.,1.));
#7009=DIRECTION('ref_axis',(1.,0.,0.));
#7010=DIRECTION('center_axis',(0.,0.,-1.));
#7011=DIRECTION('ref_axis',(1.,0.,0.));
#7012=DIRECTION('center_axis',(0.,0.,1.));
#7013=DIRECTION('ref_axis',(1.,0.,0.));
#7014=DIRECTION('',(0.,0.,-1.));
#7015=DIRECTION('center_axis',(0.,0.,1.));
#7016=DIRECTION('ref_axis',(1.,0.,0.));
#7017=DIRECTION('',(0.,0.,-1.));
#7018=DIRECTION('center_axis',(0.,0.,1.));
#7019=DIRECTION('ref_axis',(1.,0.,0.));
#7020=DIRECTION('center_axis',(0.,0.,1.));
#7021=DIRECTION('ref_axis',(1.,0.,0.));
#7022=DIRECTION('',(0.,0.,-1.));
#7023=DIRECTION('center_axis',(0.,0.,1.));
#7024=DIRECTION('ref_axis',(1.,0.,0.));
#7025=DIRECTION('axis',(0.,0.,1.));
#7026=DIRECTION('refdir',(1.,0.,0.));
#7027=DIRECTION('center_axis',(1.,0.,0.));
#7028=DIRECTION('ref_axis',(0.,0.,-1.));
#7029=DIRECTION('',(0.,0.,1.));
#7030=DIRECTION('center_axis',(1.,0.,0.));
#7031=DIRECTION('ref_axis',(0.,0.,-1.));
#7032=DIRECTION('center_axis',(1.,0.,0.));
#7033=DIRECTION('ref_axis',(0.,0.,-1.));
#7034=DIRECTION('center_axis',(1.,0.,0.));
#7035=DIRECTION('ref_axis',(0.,0.,-1.));
#7036=DIRECTION('',(1.,0.,0.));
#7037=DIRECTION('center_axis',(1.,0.,0.));
#7038=DIRECTION('ref_axis',(0.,0.,-1.));
#7039=DIRECTION('',(0.,0.,-1.));
#7040=DIRECTION('center_axis',(0.,0.,1.));
#7041=DIRECTION('ref_axis',(1.,0.,0.));
#7042=DIRECTION('center_axis',(0.,0.,-1.));
#7043=DIRECTION('ref_axis',(1.,0.,0.));
#7044=DIRECTION('',(0.,0.,-1.));
#7045=DIRECTION('center_axis',(0.,0.,-1.));
#7046=DIRECTION('ref_axis',(1.,0.,0.));
#7047=DIRECTION('center_axis',(0.,0.,1.));
#7048=DIRECTION('ref_axis',(1.,0.,0.));
#7049=DIRECTION('center_axis',(0.,0.,1.));
#7050=DIRECTION('ref_axis',(1.,0.,0.));
#7051=DIRECTION('',(0.,0.,-1.));
#7052=DIRECTION('center_axis',(0.,0.,1.));
#7053=DIRECTION('ref_axis',(1.,0.,0.));
#7054=DIRECTION('center_axis',(0.,0.,1.));
#7055=DIRECTION('ref_axis',(1.,0.,0.));
#7056=DIRECTION('center_axis',(0.,0.,1.));
#7057=DIRECTION('ref_axis',(1.,0.,0.));
#7058=DIRECTION('axis',(0.,0.,1.));
#7059=DIRECTION('refdir',(1.,0.,0.));
#7060=DIRECTION('center_axis',(0.866025403784439,0.,-0.5));
#7061=DIRECTION('ref_axis',(0.5,0.,0.866025403784439));
#7062=DIRECTION('',(0.5,0.,0.866025403784439));
#7063=DIRECTION('',(0.,-1.,0.));
#7064=DIRECTION('',(0.5,0.,0.866025403784439));
#7065=DIRECTION('',(0.,-1.,0.));
#7066=DIRECTION('center_axis',(1.92296268638356E-16,0.,-1.));
#7067=DIRECTION('ref_axis',(1.,0.,1.92296268638356E-16));
#7068=DIRECTION('',(1.,0.,1.92296268638356E-16));
#7069=DIRECTION('',(0.,-1.,0.));
#7070=DIRECTION('',(1.,0.,1.92296268638356E-16));
#7071=DIRECTION('center_axis',(-0.866025403784439,0.,-0.5));
#7072=DIRECTION('ref_axis',(0.5,0.,-0.866025403784439));
#7073=DIRECTION('',(0.5,0.,-0.866025403784439));
#7074=DIRECTION('',(0.,-1.,0.));
#7075=DIRECTION('',(0.5,0.,-0.866025403784438));
#7076=DIRECTION('center_axis',(-0.866025403784439,0.,0.5));
#7077=DIRECTION('ref_axis',(-0.5,0.,-0.866025403784439));
#7078=DIRECTION('',(-0.5,0.,-0.866025403784439));
#7079=DIRECTION('',(0.,-1.,0.));
#7080=DIRECTION('',(-0.5,0.,-0.866025403784439));
#7081=DIRECTION('center_axis',(-1.92296268638356E-16,0.,1.));
#7082=DIRECTION('ref_axis',(-1.,0.,-1.92296268638356E-16));
#7083=DIRECTION('',(-1.,0.,-1.92296268638356E-16));
#7084=DIRECTION('',(0.,-1.,0.));
#7085=DIRECTION('',(-1.,0.,-1.92296268638356E-16));
#7086=DIRECTION('center_axis',(0.866025403784439,0.,0.5));
#7087=DIRECTION('ref_axis',(-0.5,0.,0.866025403784439));
#7088=DIRECTION('',(-0.5,0.,0.866025403784439));
#7089=DIRECTION('',(-0.5,0.,0.866025403784439));
#7090=DIRECTION('center_axis',(0.,-1.,0.));
#7091=DIRECTION('ref_axis',(0.,0.,-1.));
#7092=DIRECTION('center_axis',(0.,1.,0.));
#7093=DIRECTION('ref_axis',(0.,0.,1.));
#7094=DIRECTION('center_axis',(0.,-1.,0.));
#7095=DIRECTION('ref_axis',(1.,0.,0.));
#7096=DIRECTION('center_axis',(0.,-1.,0.));
#7097=DIRECTION('ref_axis',(1.,0.,0.));
#7098=DIRECTION('center_axis',(0.,-1.,0.));
#7099=DIRECTION('ref_axis',(1.,0.,0.));
#7100=DIRECTION('',(0.707106781186547,0.707106781186548,8.65956056235493E-17));
#7101=DIRECTION('center_axis',(0.,-1.,0.));
#7102=DIRECTION('ref_axis',(1.,0.,0.));
#7103=DIRECTION('center_axis',(0.,1.,0.));
#7104=DIRECTION('ref_axis',(1.,0.,0.));
#7105=DIRECTION('',(0.,1.,0.));
#7106=DIRECTION('center_axis',(0.,1.,0.));
#7107=DIRECTION('ref_axis',(1.,0.,0.));
#7108=DIRECTION('center_axis',(0.,-1.,0.));
#7109=DIRECTION('ref_axis',(1.,0.,0.));
#7110=DIRECTION('',(-0.707106781186547,0.707106781186548,-8.65956056235493E-17));
#7111=DIRECTION('center_axis',(0.,-1.,0.));
#7112=DIRECTION('ref_axis',(0.,0.,-1.));
#7113=DIRECTION('',(0.,0.,1.));
#7114=DIRECTION('',(1.,0.,0.));
#7115=DIRECTION('',(0.,0.,1.));
#7116=DIRECTION('',(1.,0.,0.));
#7117=DIRECTION('',(0.,0.,1.));
#7118=DIRECTION('',(2.22044604925031E-16,-1.,0.));
#7119=DIRECTION('',(0.,0.,1.));
#7120=DIRECTION('',(1.,0.,0.));
#7121=DIRECTION('',(0.,0.,1.));
#7122=DIRECTION('',(1.,0.,0.));
#7123=DIRECTION('',(0.,0.,1.));
#7124=DIRECTION('',(1.,0.,0.));
#7125=CARTESIAN_POINT('',(0.,0.,0.));
#7126=CARTESIAN_POINT('',(0.,0.,0.));
#7127=CARTESIAN_POINT('',(0.,0.,0.));
#7128=CARTESIAN_POINT('Origin',(7.2,1.6,-1.1));
#7129=CARTESIAN_POINT('',(7.035,1.6,-1.));
#7130=CARTESIAN_POINT('Origin',(7.2,1.6,-1.));
#7131=CARTESIAN_POINT('',(7.035,1.6,0.));
#7132=CARTESIAN_POINT('',(7.035,1.6,-1.1));
#7133=CARTESIAN_POINT('Origin',(7.2,1.6,0.));
#7134=CARTESIAN_POINT('Origin',(7.2,-1.6,-1.1));
#7135=CARTESIAN_POINT('',(7.035,-1.6,-1.));
#7136=CARTESIAN_POINT('Origin',(7.2,-1.6,-1.));
#7137=CARTESIAN_POINT('',(7.035,-1.6,0.));
#7138=CARTESIAN_POINT('',(7.035,-1.6,-1.1));
#7139=CARTESIAN_POINT('Origin',(7.2,-1.6,0.));
#7140=CARTESIAN_POINT('Origin',(7.2,0.,-1.1));
#7141=CARTESIAN_POINT('',(6.89,-3.79640507735679E-17,-1.));
#7142=CARTESIAN_POINT('Origin',(7.2,0.,-1.));
#7143=CARTESIAN_POINT('',(6.89,3.79640507735679E-17,0.));
#7144=CARTESIAN_POINT('',(6.89,-3.79640507735679E-17,-1.1));
#7145=CARTESIAN_POINT('Origin',(7.2,0.,0.));
#7146=CARTESIAN_POINT('Origin',(-1.90918830920368,-1.90918830920368,-1.1));
#7147=CARTESIAN_POINT('',(-2.15918830920368,-1.90918830920368,-1.));
#7148=CARTESIAN_POINT('Origin',(-1.90918830920368,-1.90918830920368,-1.));
#7149=CARTESIAN_POINT('',(-2.15918830920368,-1.90918830920368,0.));
#7150=CARTESIAN_POINT('',(-2.15918830920368,-1.90918830920368,-1.1));
#7151=CARTESIAN_POINT('Origin',(-1.90918830920368,-1.90918830920368,0.));
#7152=CARTESIAN_POINT('Origin',(-1.90918830920368,1.90918830920368,-1.1));
#7153=CARTESIAN_POINT('',(-2.15918830920368,1.90918830920368,-1.));
#7154=CARTESIAN_POINT('Origin',(-1.90918830920368,1.90918830920368,-1.));
#7155=CARTESIAN_POINT('',(-2.15918830920368,1.90918830920368,0.));
#7156=CARTESIAN_POINT('',(-2.15918830920368,1.90918830920368,-1.1));
#7157=CARTESIAN_POINT('Origin',(-1.90918830920368,1.90918830920368,0.));
#7158=CARTESIAN_POINT('Origin',(1.90918830920368,1.90918830920368,-1.1));
#7159=CARTESIAN_POINT('',(1.65918830920368,1.90918830920368,-1.));
#7160=CARTESIAN_POINT('Origin',(1.90918830920368,1.90918830920368,-1.));
#7161=CARTESIAN_POINT('',(1.65918830920368,1.90918830920368,0.));
#7162=CARTESIAN_POINT('',(1.65918830920368,1.90918830920368,-1.1));
#7163=CARTESIAN_POINT('Origin',(1.90918830920368,1.90918830920368,0.));
#7164=CARTESIAN_POINT('Origin',(1.90918830920368,-1.90918830920368,-1.1));
#7165=CARTESIAN_POINT('',(1.65918830920368,-1.90918830920368,-1.));
#7166=CARTESIAN_POINT('Origin',(1.90918830920368,-1.90918830920368,-1.));
#7167=CARTESIAN_POINT('',(1.65918830920368,-1.90918830920368,0.));
#7168=CARTESIAN_POINT('',(1.65918830920368,-1.90918830920368,-1.1));
#7169=CARTESIAN_POINT('Origin',(1.90918830920368,-1.90918830920368,0.));
#7170=CARTESIAN_POINT('Origin',(10.5,10.5,-1.));
#7171=CARTESIAN_POINT('',(10.5,10.5,-1.));
#7172=CARTESIAN_POINT('',(-10.5,10.5,-1.));
#7173=CARTESIAN_POINT('',(10.5,10.5,-1.));
#7174=CARTESIAN_POINT('',(-10.5,10.5,0.));
#7175=CARTESIAN_POINT('',(-10.5,10.5,-1.));
#7176=CARTESIAN_POINT('',(10.5,10.5,0.));
#7177=CARTESIAN_POINT('',(10.5,10.5,0.));
#7178=CARTESIAN_POINT('',(10.5,10.5,-1.));
#7179=CARTESIAN_POINT('Origin',(10.5,-10.5,-1.));
#7180=CARTESIAN_POINT('',(10.5,-10.5,-1.));
#7181=CARTESIAN_POINT('',(10.5,-10.5,-1.));
#7182=CARTESIAN_POINT('',(10.5,-10.5,0.));
#7183=CARTESIAN_POINT('',(10.5,-10.5,0.));
#7184=CARTESIAN_POINT('',(10.5,-10.5,-1.));
#7185=CARTESIAN_POINT('Origin',(-10.5,-10.5,-1.));
#7186=CARTESIAN_POINT('',(-10.5,-10.5,-1.));
#7187=CARTESIAN_POINT('',(-10.5,-10.5,-1.));
#7188=CARTESIAN_POINT('',(-10.5,-10.5,0.));
#7189=CARTESIAN_POINT('',(-10.5,-10.5,0.));
#7190=CARTESIAN_POINT('',(-10.5,-10.5,-1.));
#7191=CARTESIAN_POINT('Origin',(-10.5,10.5,-1.));
#7192=CARTESIAN_POINT('',(-10.5,10.5,-1.));
#7193=CARTESIAN_POINT('',(-10.5,10.5,0.));
#7194=CARTESIAN_POINT('Origin',(0.,0.,0.));
#7195=CARTESIAN_POINT('Origin',(0.,0.,-1.));
#7196=CARTESIAN_POINT('',(0.,0.,0.));
#7197=CARTESIAN_POINT('Origin',(-9.5,-9.5,-3.5));
#7198=CARTESIAN_POINT('',(-10.5,-9.5,-1.));
#7199=CARTESIAN_POINT('Origin',(-9.5,-9.5,-1.));
#7200=CARTESIAN_POINT('',(-10.5,-9.5,-3.5));
#7201=CARTESIAN_POINT('',(-10.5,-9.5,-3.5));
#7202=CARTESIAN_POINT('Origin',(-9.5,-9.5,-3.5));
#7203=CARTESIAN_POINT('Origin',(-9.5,-9.5,-1.));
#7204=CARTESIAN_POINT('Origin',(-9.5,-9.5,-3.5));
#7205=CARTESIAN_POINT('',(0.,0.,0.));
#7206=CARTESIAN_POINT('Origin',(-9.5,9.5,-3.5));
#7207=CARTESIAN_POINT('',(-10.5,9.5,-1.));
#7208=CARTESIAN_POINT('Origin',(-9.5,9.5,-1.));
#7209=CARTESIAN_POINT('',(-10.5,9.5,-3.5));
#7210=CARTESIAN_POINT('',(-10.5,9.5,-3.5));
#7211=CARTESIAN_POINT('Origin',(-9.5,9.5,-3.5));
#7212=CARTESIAN_POINT('Origin',(-9.5,9.5,-1.));
#7213=CARTESIAN_POINT('Origin',(-9.5,9.5,-3.5));
#7214=CARTESIAN_POINT('',(0.,0.,0.));
#7215=CARTESIAN_POINT('Origin',(9.5,-9.5,-3.5));
#7216=CARTESIAN_POINT('',(8.5,-9.5,-1.));
#7217=CARTESIAN_POINT('Origin',(9.5,-9.5,-1.));
#7218=CARTESIAN_POINT('',(8.5,-9.5,-3.5));
#7219=CARTESIAN_POINT('',(8.5,-9.5,-3.5));
#7220=CARTESIAN_POINT('Origin',(9.5,-9.5,-3.5));
#7221=CARTESIAN_POINT('Origin',(9.5,-9.5,-1.));
#7222=CARTESIAN_POINT('Origin',(9.5,-9.5,-3.5));
#7223=CARTESIAN_POINT('',(0.,0.,0.));
#7224=CARTESIAN_POINT('Origin',(9.5,9.5,-3.5));
#7225=CARTESIAN_POINT('',(8.5,9.5,-1.));
#7226=CARTESIAN_POINT('Origin',(9.5,9.5,-1.));
#7227=CARTESIAN_POINT('',(8.5,9.5,-3.5));
#7228=CARTESIAN_POINT('',(8.5,9.5,-3.5));
#7229=CARTESIAN_POINT('Origin',(9.5,9.5,-3.5));
#7230=CARTESIAN_POINT('Origin',(9.5,9.5,-1.));
#7231=CARTESIAN_POINT('Origin',(9.5,9.5,-3.5));
#7232=CARTESIAN_POINT('',(0.,0.,0.));
#7233=CARTESIAN_POINT('Origin',(-1.90918830920368,-1.90918830920368,-0.1));
#7234=CARTESIAN_POINT('',(-2.23918830920368,-1.90918830920368,0.));
#7235=CARTESIAN_POINT('Origin',(-1.90918830920368,-1.90918830920368,0.));
#7236=CARTESIAN_POINT('',(-2.23918830920368,-1.90918830920368,0.8));
#7237=CARTESIAN_POINT('',(-2.23918830920368,-1.90918830920368,-0.1));
#7238=CARTESIAN_POINT('Origin',(-1.90918830920368,-1.90918830920368,0.8));
#7239=CARTESIAN_POINT('Origin',(-1.90918830920368,1.90918830920368,-0.1));
#7240=CARTESIAN_POINT('',(-2.23918830920368,1.90918830920368,0.));
#7241=CARTESIAN_POINT('Origin',(-1.90918830920368,1.90918830920368,0.));
#7242=CARTESIAN_POINT('',(-2.23918830920368,1.90918830920368,0.8));
#7243=CARTESIAN_POINT('',(-2.23918830920368,1.90918830920368,-0.1));
#7244=CARTESIAN_POINT('Origin',(-1.90918830920368,1.90918830920368,0.8));
#7245=CARTESIAN_POINT('Origin',(1.90918830920368,1.90918830920368,-0.1));
#7246=CARTESIAN_POINT('',(1.57918830920368,1.90918830920368,0.));
#7247=CARTESIAN_POINT('Origin',(1.90918830920368,1.90918830920368,0.));
#7248=CARTESIAN_POINT('',(1.57918830920368,1.90918830920368,0.8));
#7249=CARTESIAN_POINT('',(1.57918830920368,1.90918830920368,-0.1));
#7250=CARTESIAN_POINT('Origin',(1.90918830920368,1.90918830920368,0.8));
#7251=CARTESIAN_POINT('Origin',(1.90918830920368,-1.90918830920368,-0.1));
#7252=CARTESIAN_POINT('',(1.57918830920368,-1.90918830920368,0.));
#7253=CARTESIAN_POINT('Origin',(1.90918830920368,-1.90918830920368,0.));
#7254=CARTESIAN_POINT('',(1.57918830920368,-1.90918830920368,0.8));
#7255=CARTESIAN_POINT('',(1.57918830920368,-1.90918830920368,-0.1));
#7256=CARTESIAN_POINT('Origin',(1.90918830920368,-1.90918830920368,0.8));
#7257=CARTESIAN_POINT('Origin',(0.,0.,3.25));
#7258=CARTESIAN_POINT('',(-1.6,-1.95943487863577E-16,3.25));
#7259=CARTESIAN_POINT('Origin',(0.,0.,3.25));
#7260=CARTESIAN_POINT('',(-1.25,-1.53080849893419E-16,3.25));
#7261=CARTESIAN_POINT('Origin',(0.,0.,3.25));
#7262=CARTESIAN_POINT('Origin',(0.,0.,2.5));
#7263=CARTESIAN_POINT('',(-1.6,-1.95943487863577E-16,2.5));
#7264=CARTESIAN_POINT('Origin',(0.,0.,2.5));
#7265=CARTESIAN_POINT('',(-1.25,1.53080849893419E-16,2.5));
#7266=CARTESIAN_POINT('Origin',(0.,0.,2.5));
#7267=CARTESIAN_POINT('Origin',(0.,0.,2.5));
#7268=CARTESIAN_POINT('',(-1.6,-1.95943487863577E-16,2.5));
#7269=CARTESIAN_POINT('Origin',(0.,0.,0.));
#7270=CARTESIAN_POINT('',(-1.25,-1.53080849893419E-16,0.8));
#7271=CARTESIAN_POINT('',(-1.25,-1.53080849893419E-16,0.));
#7272=CARTESIAN_POINT('Origin',(0.,0.,0.8));
#7273=CARTESIAN_POINT('Origin',(0.,0.,0.8));
#7274=CARTESIAN_POINT('',(-3.5,-4.28626379701574E-16,0.8));
#7275=CARTESIAN_POINT('Origin',(0.,0.,0.8));
#7276=CARTESIAN_POINT('Origin',(0.,0.,0.));
#7277=CARTESIAN_POINT('',(-3.5,-4.28626379701574E-16,0.));
#7278=CARTESIAN_POINT('',(-3.5,-4.28626379701574E-16,0.));
#7279=CARTESIAN_POINT('Origin',(0.,0.,0.));
#7280=CARTESIAN_POINT('Origin',(0.,0.,0.));
#7281=CARTESIAN_POINT('',(-1.25,-1.53080849893419E-16,7.));
#7282=CARTESIAN_POINT('Origin',(0.,0.,7.));
#7283=CARTESIAN_POINT('',(-1.25,-1.53080849893419E-16,0.));
#7284=CARTESIAN_POINT('Origin',(0.,0.,7.));
#7285=CARTESIAN_POINT('Origin',(0.,0.,0.));
#7286=CARTESIAN_POINT('',(0.,0.,0.));
#7287=CARTESIAN_POINT('Origin',(0.,0.,4.75));
#7288=CARTESIAN_POINT('',(-1.255,-1.53693173292993E-16,6.25));
#7289=CARTESIAN_POINT('Origin',(0.,0.,6.25));
#7290=CARTESIAN_POINT('',(-1.255,-1.53693173292993E-16,4.75));
#7291=CARTESIAN_POINT('',(-1.255,-1.53693173292993E-16,4.75));
#7292=CARTESIAN_POINT('Origin',(0.,0.,4.75));
#7293=CARTESIAN_POINT('Origin',(0.,0.,4.75));
#7294=CARTESIAN_POINT('',(-1.7,-2.0818995585505E-16,6.25));
#7295=CARTESIAN_POINT('Origin',(0.,0.,6.25));
#7296=CARTESIAN_POINT('',(-1.7,-2.0818995585505E-16,4.75));
#7297=CARTESIAN_POINT('',(-1.7,-2.0818995585505E-16,4.75));
#7298=CARTESIAN_POINT('Origin',(0.,0.,4.75));
#7299=CARTESIAN_POINT('Origin',(0.,0.,6.25));
#7300=CARTESIAN_POINT('Origin',(0.,0.,4.75));
#7301=CARTESIAN_POINT('',(0.,0.,0.));
#7302=CARTESIAN_POINT('Origin',(1.24,0.,6.6));
#7303=CARTESIAN_POINT('',(1.24,0.19345542122153,6.51829932680816));
#7304=CARTESIAN_POINT('',(1.24,0.19345542122153,6.68170067319184));
#7305=CARTESIAN_POINT('',(1.24,0.193455421221531,6.25));
#7306=CARTESIAN_POINT('Origin',(1.24,0.,6.6));
#7307=CARTESIAN_POINT('Origin',(1.24,0.,6.6));
#7308=CARTESIAN_POINT('',(1.24,-0.19345542122153,6.51829932680816));
#7309=CARTESIAN_POINT('Ctrl Pts',(1.24,-0.193455421221531,6.51829932680816));
#7310=CARTESIAN_POINT('Ctrl Pts',(1.24167145707784,-0.182741806873435,6.49293103184137));
#7311=CARTESIAN_POINT('Ctrl Pts',(1.24400210952839,-0.16680484953796,6.46982000143961));
#7312=CARTESIAN_POINT('Ctrl Pts',(1.24840249136865,-0.129875785635207,6.43289093753686));
#7313=CARTESIAN_POINT('Ctrl Pts',(1.2507589672592,-0.106295060941802,6.4167372734261));
#7314=CARTESIAN_POINT('Ctrl Pts',(1.25408084670822,-0.0545698089447939,
6.39529044194989));
#7315=CARTESIAN_POINT('Ctrl Pts',(1.255,-0.0264211917910691,6.39));
#7316=CARTESIAN_POINT('Ctrl Pts',(1.255,0.026421191791069,6.39));
#7317=CARTESIAN_POINT('Ctrl Pts',(1.25408084670822,0.0545698089447938,6.39529044194989));
#7318=CARTESIAN_POINT('Ctrl Pts',(1.2507589672592,0.106295060941802,6.4167372734261));
#7319=CARTESIAN_POINT('Ctrl Pts',(1.24840249136865,0.129875785635207,6.43289093753686));
#7320=CARTESIAN_POINT('Ctrl Pts',(1.24400210952839,0.166804849537961,6.46982000143961));
#7321=CARTESIAN_POINT('Ctrl Pts',(1.24167145707784,0.182741806873435,6.49293103184137));
#7322=CARTESIAN_POINT('Ctrl Pts',(1.24,0.193455421221531,6.51829932680816));
#7323=CARTESIAN_POINT('',(1.24,-0.19345542122153,6.68170067319184));
#7324=CARTESIAN_POINT('Origin',(1.24,0.,6.6));
#7325=CARTESIAN_POINT('',(1.255,-5.44921548144906E-17,6.81));
#7326=CARTESIAN_POINT('Ctrl Pts',(1.255,-3.46944695195361E-17,6.81));
#7327=CARTESIAN_POINT('Ctrl Pts',(1.255,-0.0264211917910691,6.81));
#7328=CARTESIAN_POINT('Ctrl Pts',(1.25408084670822,-0.0545698089447938,
6.80470955805011));
#7329=CARTESIAN_POINT('Ctrl Pts',(1.2507589672592,-0.106295060941802,6.7832627265739));
#7330=CARTESIAN_POINT('Ctrl Pts',(1.24840249136865,-0.129875785635207,6.76710906246314));
#7331=CARTESIAN_POINT('Ctrl Pts',(1.24400210952839,-0.166804849537961,6.73017999856039));
#7332=CARTESIAN_POINT('Ctrl Pts',(1.24167145707784,-0.182741806873434,6.70706896815863));
#7333=CARTESIAN_POINT('Ctrl Pts',(1.24,-0.193455421221531,6.68170067319184));
#7334=CARTESIAN_POINT('',(1.8,-2.57175827820944E-17,6.81));
#7335=CARTESIAN_POINT('',(1.24,-2.57175827820944E-17,6.81));
#7336=CARTESIAN_POINT('',(1.78770802985275,0.21,6.6));
#7337=CARTESIAN_POINT('Ctrl Pts',(1.78770802985275,0.21,6.6));
#7338=CARTESIAN_POINT('Ctrl Pts',(1.78770802985275,0.21,6.57360603148425));
#7339=CARTESIAN_POINT('Ctrl Pts',(1.78835284034214,0.204720232951726,6.54546934556601));
#7340=CARTESIAN_POINT('Ctrl Pts',(1.79067700538683,0.1832815239789,6.49373688397397));
#7341=CARTESIAN_POINT('Ctrl Pts',(1.79232226897314,0.167123888882363,6.47013904078401));
#7342=CARTESIAN_POINT('Ctrl Pts',(1.79540680803063,0.129861077103665,6.43287622900531));
#7343=CARTESIAN_POINT('Ctrl Pts',(1.79704717240673,0.106263182528071,6.4167185016358));
#7344=CARTESIAN_POINT('Ctrl Pts',(1.79936011492601,0.0545305475112077,6.39527972468261));
#7345=CARTESIAN_POINT('Ctrl Pts',(1.8,0.0263938015120406,6.39));
#7346=CARTESIAN_POINT('Ctrl Pts',(1.8,-0.0263938015120406,6.39));
#7347=CARTESIAN_POINT('Ctrl Pts',(1.79936011492601,-0.0545305475112077,
6.39527972468261));
#7348=CARTESIAN_POINT('Ctrl Pts',(1.79704717240673,-0.106263182528071,6.4167185016358));
#7349=CARTESIAN_POINT('Ctrl Pts',(1.79540680803063,-0.129861077103665,6.43287622900531));
#7350=CARTESIAN_POINT('Ctrl Pts',(1.79232226897314,-0.167123888882363,6.47013904078401));
#7351=CARTESIAN_POINT('Ctrl Pts',(1.79067700538683,-0.1832815239789,6.49373688397397));
#7352=CARTESIAN_POINT('Ctrl Pts',(1.78835284034214,-0.204720232951726,6.54546934556602));
#7353=CARTESIAN_POINT('Ctrl Pts',(1.78770802985275,-0.21,6.57360603148425));
#7354=CARTESIAN_POINT('Ctrl Pts',(1.78770802985275,-0.21,6.62639396851575));
#7355=CARTESIAN_POINT('Ctrl Pts',(1.78835284034214,-0.204720232951726,6.65453065443398));
#7356=CARTESIAN_POINT('Ctrl Pts',(1.79067700538683,-0.1832815239789,6.70626311602603));
#7357=CARTESIAN_POINT('Ctrl Pts',(1.79232226897314,-0.167123888882363,6.72986095921599));
#7358=CARTESIAN_POINT('Ctrl Pts',(1.79540680803063,-0.129861077103665,6.76712377099468));
#7359=CARTESIAN_POINT('Ctrl Pts',(1.79704717240673,-0.106263182528071,6.7832814983642));
#7360=CARTESIAN_POINT('Ctrl Pts',(1.79936011492601,-0.0545305475112076,
6.80472027531739));
#7361=CARTESIAN_POINT('Ctrl Pts',(1.8,-0.0263938015120407,6.81));
#7362=CARTESIAN_POINT('Ctrl Pts',(1.8,-6.93889390390723E-17,6.81));
#7363=CARTESIAN_POINT('Ctrl Pts',(1.8,-2.77555756156289E-17,6.81));
#7364=CARTESIAN_POINT('Ctrl Pts',(1.8,0.0263938015120406,6.81));
#7365=CARTESIAN_POINT('Ctrl Pts',(1.79936011492601,0.0545305475112076,6.80472027531739));
#7366=CARTESIAN_POINT('Ctrl Pts',(1.79704717240673,0.106263182528071,6.7832814983642));
#7367=CARTESIAN_POINT('Ctrl Pts',(1.79540680803063,0.129861077103665,6.76712377099468));
#7368=CARTESIAN_POINT('Ctrl Pts',(1.79232226897314,0.167123888882363,6.72986095921599));
#7369=CARTESIAN_POINT('Ctrl Pts',(1.79067700538683,0.1832815239789,6.70626311602603));
#7370=CARTESIAN_POINT('Ctrl Pts',(1.78835284034214,0.204720232951726,6.65453065443398));
#7371=CARTESIAN_POINT('Ctrl Pts',(1.78770802985275,0.21,6.62639396851575));
#7372=CARTESIAN_POINT('Ctrl Pts',(1.78770802985275,0.21,6.6));
#7373=CARTESIAN_POINT('Ctrl Pts',(1.24,0.193455421221531,6.68170067319184));
#7374=CARTESIAN_POINT('Ctrl Pts',(1.24167145707784,0.182741806873435,6.70706896815863));
#7375=CARTESIAN_POINT('Ctrl Pts',(1.24400210952839,0.166804849537961,6.73017999856039));
#7376=CARTESIAN_POINT('Ctrl Pts',(1.24840249136865,0.129875785635207,6.76710906246314));
#7377=CARTESIAN_POINT('Ctrl Pts',(1.2507589672592,0.106295060941802,6.7832627265739));
#7378=CARTESIAN_POINT('Ctrl Pts',(1.25408084670822,0.0545698089447938,6.80470955805011));
#7379=CARTESIAN_POINT('Ctrl Pts',(1.255,0.0264211917910689,6.81));
#7380=CARTESIAN_POINT('Ctrl Pts',(1.255,-8.32667268468867E-17,6.81));
#7381=CARTESIAN_POINT('Origin',(1.24,0.,6.6));
#7382=CARTESIAN_POINT('',(1.24,-0.193455421221531,6.25));
#7383=CARTESIAN_POINT('Origin',(0.,0.,6.25));
#7384=CARTESIAN_POINT('',(-1.255,-1.53693173292993E-16,7.));
#7385=CARTESIAN_POINT('Origin',(0.,0.,7.));
#7386=CARTESIAN_POINT('',(-1.255,-1.53693173292993E-16,6.25));
#7387=CARTESIAN_POINT('',(-1.255,-1.53693173292993E-16,6.25));
#7388=CARTESIAN_POINT('Origin',(0.,0.,6.25));
#7389=CARTESIAN_POINT('Origin',(0.,0.,6.25));
#7390=CARTESIAN_POINT('',(-1.8,-2.20436423846524E-16,7.));
#7391=CARTESIAN_POINT('Origin',(0.,0.,7.));
#7392=CARTESIAN_POINT('',(-1.8,-2.20436423846524E-16,6.25));
#7393=CARTESIAN_POINT('',(-1.8,-2.20436423846524E-16,6.25));
#7394=CARTESIAN_POINT('Origin',(0.,0.,6.25));
#7395=CARTESIAN_POINT('Origin',(0.,0.,7.));
#7396=CARTESIAN_POINT('Origin',(0.,0.,6.25));
#7397=CARTESIAN_POINT('',(0.,0.,0.));
#7398=CARTESIAN_POINT('Origin',(7.2,1.6,-0.1));
#7399=CARTESIAN_POINT('',(6.975,1.6,0.));
#7400=CARTESIAN_POINT('Origin',(7.2,1.6,0.));
#7401=CARTESIAN_POINT('',(6.975,1.6,1.));
#7402=CARTESIAN_POINT('',(6.975,1.6,-0.1));
#7403=CARTESIAN_POINT('Origin',(7.2,1.6,1.));
#7404=CARTESIAN_POINT('Origin',(7.2,-1.6,-0.1));
#7405=CARTESIAN_POINT('',(6.975,-1.6,0.));
#7406=CARTESIAN_POINT('Origin',(7.2,-1.6,0.));
#7407=CARTESIAN_POINT('',(6.975,-1.6,1.));
#7408=CARTESIAN_POINT('',(6.975,-1.6,-0.1));
#7409=CARTESIAN_POINT('Origin',(7.2,-1.6,1.));
#7410=CARTESIAN_POINT('Origin',(7.2,0.,0.5));
#7411=CARTESIAN_POINT('',(6.2,-1.22464679914735E-16,0.5));
#7412=CARTESIAN_POINT('Origin',(7.2,0.,0.5));
#7413=CARTESIAN_POINT('',(6.2,1.22464679914735E-16,1.));
#7414=CARTESIAN_POINT('',(6.2,-1.22464679914735E-16,0.5));
#7415=CARTESIAN_POINT('Origin',(7.2,0.,1.));
#7416=CARTESIAN_POINT('Origin',(7.2,0.,0.5));
#7417=CARTESIAN_POINT('',(6.89,-3.79640507735679E-17,0.5));
#7418=CARTESIAN_POINT('Origin',(7.2,0.,0.5));
#7419=CARTESIAN_POINT('Origin',(7.2,0.,0.));
#7420=CARTESIAN_POINT('',(6.89,-3.79640507735679E-17,0.));
#7421=CARTESIAN_POINT('',(6.89,-3.79640507735679E-17,0.));
#7422=CARTESIAN_POINT('Origin',(7.2,0.,0.));
#7423=CARTESIAN_POINT('Origin',(7.2,0.,0.));
#7424=CARTESIAN_POINT('',(5.2,-2.44929359829471E-16,1.));
#7425=CARTESIAN_POINT('Origin',(7.2,0.,1.));
#7426=CARTESIAN_POINT('',(5.2,-2.44929359829471E-16,0.));
#7427=CARTESIAN_POINT('',(5.2,-2.44929359829471E-16,0.));
#7428=CARTESIAN_POINT('Origin',(7.2,0.,0.));
#7429=CARTESIAN_POINT('Origin',(7.2,0.,1.));
#7430=CARTESIAN_POINT('Origin',(7.2,0.,0.));
#7431=CARTESIAN_POINT('',(0.,0.,0.));
#7432=CARTESIAN_POINT('Origin',(7.2,0.,5.));
#7433=CARTESIAN_POINT('',(6.89,-3.79640507735679E-17,5.7));
#7434=CARTESIAN_POINT('Origin',(7.2,0.,5.7));
#7435=CARTESIAN_POINT('',(6.89,-3.79640507735679E-17,5.));
#7436=CARTESIAN_POINT('',(6.89,-3.79640507735679E-17,5.));
#7437=CARTESIAN_POINT('Origin',(7.2,0.,5.));
#7438=CARTESIAN_POINT('Origin',(7.2,0.,5.));
#7439=CARTESIAN_POINT('',(6.6,-7.34788079488412E-17,5.));
#7440=CARTESIAN_POINT('Origin',(7.2,0.,5.));
#7441=CARTESIAN_POINT('Origin',(7.2,0.,0.5));
#7442=CARTESIAN_POINT('',(6.6,-7.34788079488412E-17,0.5));
#7443=CARTESIAN_POINT('',(6.6,-7.34788079488412E-17,0.5));
#7444=CARTESIAN_POINT('Origin',(7.2,0.,0.5));
#7445=CARTESIAN_POINT('Origin',(7.2,0.,0.5));
#7446=CARTESIAN_POINT('',(6.2,-1.22464679914735E-16,5.7));
#7447=CARTESIAN_POINT('Origin',(7.2,0.,5.7));
#7448=CARTESIAN_POINT('',(6.2,-1.22464679914735E-16,0.5));
#7449=CARTESIAN_POINT('',(6.2,-1.22464679914735E-16,0.5));
#7450=CARTESIAN_POINT('Origin',(7.2,0.,0.5));
#7451=CARTESIAN_POINT('Origin',(7.2,0.,5.7));
#7452=CARTESIAN_POINT('Origin',(7.2,0.,0.5));
#7453=CARTESIAN_POINT('',(0.,0.,0.));
#7454=CARTESIAN_POINT('Ctrl Pts',(7.64999870073278,0.00963880430002493,
0.500937861339137));
#7455=CARTESIAN_POINT('Ctrl Pts',(7.64999072283273,0.0688240253405825,0.512565458280486));
#7456=CARTESIAN_POINT('Ctrl Pts',(7.62651906829351,0.186933280416436,0.535860737255745));
#7457=CARTESIAN_POINT('Ctrl Pts',(7.52538952050926,0.338721501716328,0.571111621876026));
#7458=CARTESIAN_POINT('Ctrl Pts',(7.37261016576107,0.440828782725881,0.606632113855559));
#7459=CARTESIAN_POINT('Ctrl Pts',(7.19098801918939,0.477160089388571,0.642432691908446));
#7460=CARTESIAN_POINT('Ctrl Pts',(7.00794887133667,0.440792445335284,0.678501299793522));
#7461=CARTESIAN_POINT('Ctrl Pts',(6.85151949944076,0.336499171833787,0.714833893830788));
#7462=CARTESIAN_POINT('Ctrl Pts',(6.74635289761356,0.179164878106423,0.751420068859459));
#7463=CARTESIAN_POINT('Ctrl Pts',(6.7088855037237,-0.00779582609077112,
0.78825059826266));
#7464=CARTESIAN_POINT('Ctrl Pts',(6.74651391108833,-0.195622387289353,0.825313313466632));
#7465=CARTESIAN_POINT('Ctrl Pts',(6.88851119015049,-0.410310488976418,0.875022999496246));
#7466=CARTESIAN_POINT('Ctrl Pts',(7.20522985356176,-0.542753193552164,0.937673401670968));
#7467=CARTESIAN_POINT('Ctrl Pts',(7.52560124560565,-0.410308950963103,1.00090311405878));
#7468=CARTESIAN_POINT('Ctrl Pts',(7.67086762315913,-0.190619832396083,1.0517623380234));
#7469=CARTESIAN_POINT('Ctrl Pts',(7.72038428103372,0.053554354178951,1.09994516441643));
#7470=CARTESIAN_POINT('Ctrl Pts',(7.61346157902179,0.349425527858921,1.15825605943124));
#7471=CARTESIAN_POINT('Ctrl Pts',(7.293147036645,0.533923363778534,1.22671892603372));
#7472=CARTESIAN_POINT('Ctrl Pts',(6.9598052915743,0.475238618295502,1.28954716027338));
#7473=CARTESIAN_POINT('Ctrl Pts',(6.74803078150055,0.262318163018047,1.34663189357301));
#7474=CARTESIAN_POINT('Ctrl Pts',(6.67830810206772,0.0023988076890563,1.3979329504908));
#7475=CARTESIAN_POINT('Ctrl Pts',(6.74786353789082,-0.257385664114871,1.44910892564238));
#7476=CARTESIAN_POINT('Ctrl Pts',(6.93745136291826,-0.446625861944449,1.50011118169226));
#7477=CARTESIAN_POINT('Ctrl Pts',(7.19511270617401,-0.515530236866011,1.55089291586215));
#7478=CARTESIAN_POINT('Ctrl Pts',(7.45136837615866,-0.446648689171563,1.60140954707133));
#7479=CARTESIAN_POINT('Ctrl Pts',(7.63768442718454,-0.260018056286165,1.65161922462518));
#7480=CARTESIAN_POINT('Ctrl Pts',(7.70523033687804,-0.0069714683683192,
1.70148323387221));
#7481=CARTESIAN_POINT('Ctrl Pts',(7.63769895751989,0.244003419049979,1.75096640161628));
#7482=CARTESIAN_POINT('Ctrl Pts',(7.45523859330254,0.426040600914326,1.80003745460796));
#7483=CARTESIAN_POINT('Ctrl Pts',(7.20843773134158,0.491855409637758,1.84866933496872));
#7484=CARTESIAN_POINT('Ctrl Pts',(6.96411419073211,0.426044527968114,1.89683949153479));
#7485=CARTESIAN_POINT('Ctrl Pts',(6.7872702247347,0.248717255937941,1.94453007704133));
#7486=CARTESIAN_POINT('Ctrl Pts',(6.72333142706999,0.00910740273079913,
1.99172820696913));
#7487=CARTESIAN_POINT('Ctrl Pts',(6.77669190792476,-0.188112629887261,2.03064296753181));
#7488=CARTESIAN_POINT('Ctrl Pts',(6.87311288530633,-0.313353108724919,2.06152326719269));
#7489=CARTESIAN_POINT('Ctrl Pts',(6.9977575234091,-0.409174440391491,2.0922362142172));
#7490=CARTESIAN_POINT('Ctrl Pts',(7.19095586866206,-0.460713817161615,2.13031448846159));
#7491=CARTESIAN_POINT('Ctrl Pts',(7.42021304552618,-0.399036009194613,2.17551521533059));
#7492=CARTESIAN_POINT('Ctrl Pts',(7.58607675038944,-0.232652998639623,2.22023530187249));
#7493=CARTESIAN_POINT('Ctrl Pts',(7.64084113722653,-0.0267711157317457,
2.2608041635776));
#7494=CARTESIAN_POINT('Ctrl Pts',(7.60365245023964,0.158696418911201,2.2973634945418));
#7495=CARTESIAN_POINT('Ctrl Pts',(7.50973838584388,0.299219822341778,2.33003006433835));
#7496=CARTESIAN_POINT('Ctrl Pts',(7.37007100234203,0.392281683236922,2.36247215334549));
#7497=CARTESIAN_POINT('Ctrl Pts',(7.18832364110351,0.428509871500047,2.39828479951764));
#7498=CARTESIAN_POINT('Ctrl Pts',(6.98993152312495,0.375130255900093,2.43739940337039));
#7499=CARTESIAN_POINT('Ctrl Pts',(6.83283942785452,0.217642962930976,2.47976008769737));
#7500=CARTESIAN_POINT('Ctrl Pts',(6.7805179762894,0.0217759129571612,2.51834494637949));
#7501=CARTESIAN_POINT('Ctrl Pts',(6.81611962546049,-0.155110783437508,2.55325894844757));
#7502=CARTESIAN_POINT('Ctrl Pts',(6.93559514558806,-0.335467183812974,2.59501419582854));
#7503=CARTESIAN_POINT('Ctrl Pts',(7.19838636703693,-0.444497554803198,2.64699296075227));
#7504=CARTESIAN_POINT('Ctrl Pts',(7.51396784981042,-0.313675439428632,2.70919005501935));
#7505=CARTESIAN_POINT('Ctrl Pts',(7.62212313812957,-0.0514208051434247,
2.76101600110827));
#7506=CARTESIAN_POINT('Ctrl Pts',(7.57941022831611,0.159498854704775,2.80255943176652));
#7507=CARTESIAN_POINT('Ctrl Pts',(7.49002790476542,0.293811387305209,2.83377939972915));
#7508=CARTESIAN_POINT('Ctrl Pts',(7.3552499441484,0.383795703607156,2.86508254302445));
#7509=CARTESIAN_POINT('Ctrl Pts',(7.19595280633545,0.41560735445773,2.89648910888395));
#7510=CARTESIAN_POINT('Ctrl Pts',(7.03593949389396,0.383792650446306,2.92801879141503));
#7511=CARTESIAN_POINT('Ctrl Pts',(6.89961651509014,0.292876470296345,2.95969053299985));
#7512=CARTESIAN_POINT('Ctrl Pts',(6.8081238548802,0.155952445855146,2.99152250722056));
#7513=CARTESIAN_POINT('Ctrl Pts',(6.7719951154116,-0.0244720795860329,3.02708849903104));
#7514=CARTESIAN_POINT('Ctrl Pts',(6.82508694038131,-0.224423780156864,3.0664872528009));
#7515=CARTESIAN_POINT('Ctrl Pts',(6.9861130399098,-0.385566648672682,3.1098474493302));
#7516=CARTESIAN_POINT('Ctrl Pts',(7.18949761386412,-0.440411898981026,3.14997109794484));
#7517=CARTESIAN_POINT('Ctrl Pts',(7.37626527013998,-0.403213775048244,3.18676673081186));
#7518=CARTESIAN_POINT('Ctrl Pts',(7.51993103796524,-0.30750405465344,3.2201390303787));
#7519=CARTESIAN_POINT('Ctrl Pts',(7.61665044076158,-0.16281791922389,3.25377599756719));
#7520=CARTESIAN_POINT('Ctrl Pts',(7.65498225700094,0.0283123086785322,3.29145196922942));
#7521=CARTESIAN_POINT('Ctrl Pts',(7.59852316170633,0.240631420079613,3.3332902111484));
#7522=CARTESIAN_POINT('Ctrl Pts',(7.42736589163809,0.412328652603764,3.37943210760514));
#7523=CARTESIAN_POINT('Ctrl Pts',(7.19081184831391,0.475941162716025,3.42607713455886));
#7524=CARTESIAN_POINT('Ctrl Pts',(6.95151342469985,0.412204069493947,3.47322302929114));
#7525=CARTESIAN_POINT('Ctrl Pts',(6.77437422620912,0.235528496642651,3.52086247665056));
#7526=CARTESIAN_POINT('Ctrl Pts',(6.70856719057301,-0.00853695568196444,
3.56898306053165));
#7527=CARTESIAN_POINT('Ctrl Pts',(6.77444746404088,-0.255049338492359,3.61756749823055));
#7528=CARTESIAN_POINT('Ctrl Pts',(6.9562898685306,-0.437346140614658,3.66659366870206));
#7529=CARTESIAN_POINT('Ctrl Pts',(7.20705837195632,-0.504822359013845,3.71603499825878));
#7530=CARTESIAN_POINT('Ctrl Pts',(7.45987118758895,-0.437340247483335,3.76586064283255));
#7531=CARTESIAN_POINT('Ctrl Pts',(7.64643847266503,-0.251145802482984,3.81603581337119));
#7532=CARTESIAN_POINT('Ctrl Pts',(7.70939130979041,-0.0164226811455054,
3.86231497498143));
#7533=CARTESIAN_POINT('Ctrl Pts',(7.66665300702434,0.198091300428752,3.90458351454994));
#7534=CARTESIAN_POINT('Ctrl Pts',(7.55703831361006,0.362363180751678,3.94275824199772));
#7535=CARTESIAN_POINT('Ctrl Pts',(7.39231161872226,0.472405147713809,3.98104671473859));
#7536=CARTESIAN_POINT('Ctrl Pts',(7.19757748614764,0.511253819560404,4.01942894411337));
#7537=CARTESIAN_POINT('Ctrl Pts',(7.00243742159468,0.472394913482402,4.05788442705078));
#7538=CARTESIAN_POINT('Ctrl Pts',(6.83675859423202,0.361776141956741,4.09639221672569));
#7539=CARTESIAN_POINT('Ctrl Pts',(6.72593678453896,0.195994806221917,4.13493108529455));
#7540=CARTESIAN_POINT('Ctrl Pts',(6.6870196897812,0.000372767277272366,
4.17347960299015));
#7541=CARTESIAN_POINT('Ctrl Pts',(6.72599808190112,-0.19515902350661,4.21201632288769));
#7542=CARTESIAN_POINT('Ctrl Pts',(6.83662574734572,-0.360840864201945,4.25051978478148));
#7543=CARTESIAN_POINT('Ctrl Pts',(7.00208504736442,-0.47127212461887,4.28896891774833));
#7544=CARTESIAN_POINT('Ctrl Pts',(7.19679737636779,-0.510060779189973,4.32734248506513));
#7545=CARTESIAN_POINT('Ctrl Pts',(7.39100313831524,-0.471299286801184,4.36562087591661));
#7546=CARTESIAN_POINT('Ctrl Pts',(7.5551719819179,-0.361667391724164,4.40378216412631));
#7547=CARTESIAN_POINT('Ctrl Pts',(7.66435033350436,-0.197951056928272,4.44181269280615));
#7548=CARTESIAN_POINT('Ctrl Pts',(7.68982126235038,-0.0699660743691742,
4.46705762798012));
#7549=CARTESIAN_POINT('Ctrl Pts',(7.68982990724746,-0.00583191542195246,
4.4796574990714));
#7550=CARTESIAN_POINT('Ctrl Pts',(7.6350387358516,0.00963678776443446,0.500937861339137));
#7551=CARTESIAN_POINT('Ctrl Pts',(7.63503101014841,0.0669510493656743,0.512197887426284));
#7552=CARTESIAN_POINT('Ctrl Pts',(7.61231574924475,0.1812935300152,0.5347473807854));
#7553=CARTESIAN_POINT('Ctrl Pts',(7.51437536109004,0.328330400226009,0.568888525111363));
#7554=CARTESIAN_POINT('Ctrl Pts',(7.36630661624771,0.427307066398246,0.603312533918598));
#7555=CARTESIAN_POINT('Ctrl Pts',(7.19013369937419,0.462570873330364,0.638036216400197));
#7556=CARTESIAN_POINT('Ctrl Pts',(7.01240713420346,0.42727728453773,0.673054009319043));
#7557=CARTESIAN_POINT('Ctrl Pts',(6.86033508130397,0.325921179563573,0.70836726659389));
#7558=CARTESIAN_POINT('Ctrl Pts',(6.7579611971146,0.172802978923407,0.74397206566071));
#7559=CARTESIAN_POINT('Ctrl Pts',(6.7214123199082,-0.00940771975300016,
0.779864408487187));
#7560=CARTESIAN_POINT('Ctrl Pts',(6.7581198571664,-0.192756797259193,0.816037450325855));
#7561=CARTESIAN_POINT('Ctrl Pts',(6.89690232809005,-0.402672103199899,0.86463407058812));
#7562=CARTESIAN_POINT('Ctrl Pts',(7.20725605051053,-0.532709504267443,0.926031233812609));
#7563=CARTESIAN_POINT('Ctrl Pts',(7.52258283785506,-0.402635707082477,0.988237247131344));
#7564=CARTESIAN_POINT('Ctrl Pts',(7.66601723416036,-0.185829339954806,1.0384238006937));
#7565=CARTESIAN_POINT('Ctrl Pts',(7.71503355357269,0.0556422780873975,1.08607199043942));
#7566=CARTESIAN_POINT('Ctrl Pts',(7.60918637088204,0.349162880547258,1.14388762640479));
#7567=CARTESIAN_POINT('Ctrl Pts',(7.2903515128854,0.533103613911741,1.21204744313397));
#7568=CARTESIAN_POINT('Ctrl Pts',(6.95707366748621,0.474656316327783,1.27485358832891));
#7569=CARTESIAN_POINT('Ctrl Pts',(6.74456178112433,0.261169820551568,1.33209897131474));
#7570=CARTESIAN_POINT('Ctrl Pts',(6.67433527221315,-0.000269397014741131,
1.38369681229794));
#7571=CARTESIAN_POINT('Ctrl Pts',(6.74440593081803,-0.262373809003338,1.43532105174058));
#7572=CARTESIAN_POINT('Ctrl Pts',(6.93612728066397,-0.453872081669123,1.48690459984704));
#7573=CARTESIAN_POINT('Ctrl Pts',(7.19745122001508,-0.523848922372219,1.53840681076736));
#7574=CARTESIAN_POINT('Ctrl Pts',(7.45805997886714,-0.453883269663763,1.58977025772498));
#7575=CARTESIAN_POINT('Ctrl Pts',(7.64803983262086,-0.263693101035238,1.64094678753314));
#7576=CARTESIAN_POINT('Ctrl Pts',(7.71711952609534,-0.00517849878257243,
1.69188667453881));
#7577=CARTESIAN_POINT('Ctrl Pts',(7.64804216604535,0.251791239903175,1.74254418096352));
#7578=CARTESIAN_POINT('Ctrl Pts',(7.46092188629594,0.438558185201571,1.79287579243366));
#7579=CARTESIAN_POINT('Ctrl Pts',(7.20735063505956,0.506228936588262,1.8428415890961));
#7580=CARTESIAN_POINT('Ctrl Pts',(6.95593925559357,0.438549903941295,1.89240539488024));
#7581=CARTESIAN_POINT('Ctrl Pts',(6.77373440484268,0.255889979988123,1.94153491121713));
#7582=CARTESIAN_POINT('Ctrl Pts',(6.70778531151454,0.00882356266419227,
1.99020293693628));
#7583=CARTESIAN_POINT('Ctrl Pts',(6.76283355713105,-0.194668074958629,2.0303550609426));
#7584=CARTESIAN_POINT('Ctrl Pts',(6.86234426891409,-0.323919294450078,2.06222522567205));
#7585=CARTESIAN_POINT('Ctrl Pts',(6.99099241075521,-0.4228168735756,2.09392553998431));
#7586=CARTESIAN_POINT('Ctrl Pts',(7.19040501251761,-0.476002229606067,2.1332315590035));
#7587=CARTESIAN_POINT('Ctrl Pts',(7.42694509743174,-0.412343436770496,2.17987197648186));
#7588=CARTESIAN_POINT('Ctrl Pts',(7.59795477669367,-0.24075224108209,2.22599099832676));
#7589=CARTESIAN_POINT('Ctrl Pts',(7.65432879696381,-0.0286540038200118,
2.26778999749925));
#7590=CARTESIAN_POINT('Ctrl Pts',(7.61604593360169,0.162166641626849,2.30540718503675));
#7591=CARTESIAN_POINT('Ctrl Pts',(7.51950918270181,0.306566623965249,2.33898210158965));
#7592=CARTESIAN_POINT('Ctrl Pts',(7.37615986978507,0.402052531958415,2.3722797613854));
#7593=CARTESIAN_POINT('Ctrl Pts',(7.18991757189564,0.439140491267482,2.40898011568004));
#7594=CARTESIAN_POINT('Ctrl Pts',(6.98704945595601,0.384483438050293,2.44898977868643));
#7595=CARTESIAN_POINT('Ctrl Pts',(6.82687936658702,0.223795186966439,2.49220010365028));
#7596=CARTESIAN_POINT('Ctrl Pts',(6.77374406457618,0.0245525470923147,2.53145813471135));
#7597=CARTESIAN_POINT('Ctrl Pts',(6.80989272676198,-0.154854651698435,2.56687895662991));
#7598=CARTESIAN_POINT('Ctrl Pts',(6.93084711889443,-0.337336060775077,2.60913936898076));
#7599=CARTESIAN_POINT('Ctrl Pts',(7.19586714485277,-0.446979863060233,2.66154817199395));
#7600=CARTESIAN_POINT('Ctrl Pts',(7.51214995264661,-0.315456586630328,2.72392487242511));
#7601=CARTESIAN_POINT('Ctrl Pts',(7.61973089828985,-0.0538169044635309,
2.77562308796219));
#7602=CARTESIAN_POINT('Ctrl Pts',(7.57725516276559,0.155639272831775,2.81688936140585));
#7603=CARTESIAN_POINT('Ctrl Pts',(7.48867898425771,0.288669487348,2.84782028505493));
#7604=CARTESIAN_POINT('Ctrl Pts',(7.35549434227958,0.377544841875494,2.8787535369846));
#7605=CARTESIAN_POINT('Ctrl Pts',(7.19848583194038,0.408858679622143,2.90971124099487));
#7606=CARTESIAN_POINT('Ctrl Pts',(7.0411630337891,0.37754703996107,2.94071683444724));
#7607=CARTESIAN_POINT('Ctrl Pts',(6.90744882895457,0.288327999365551,2.97179002108998));
#7608=CARTESIAN_POINT('Ctrl Pts',(6.8179071425464,0.154275853325778,3.00295604846018));
#7609=CARTESIAN_POINT('Ctrl Pts',(6.78264236297597,-0.0220015791954167,
3.03770458582966));
#7610=CARTESIAN_POINT('Ctrl Pts',(6.8344572243931,-0.216935347146573,3.07612357321105));
#7611=CARTESIAN_POINT('Ctrl Pts',(6.99115063676539,-0.373674687144112,3.11831302609281));
#7612=CARTESIAN_POINT('Ctrl Pts',(7.18868631032597,-0.426903740536407,3.15728375484868));
#7613=CARTESIAN_POINT('Ctrl Pts',(7.36984365698281,-0.390811492032386,3.19297776573814));
#7614=CARTESIAN_POINT('Ctrl Pts',(7.50907371772657,-0.298044602028427,3.22532144483156));
#7615=CARTESIAN_POINT('Ctrl Pts',(7.60274490909148,-0.15791000624285,3.2579014410467));
#7616=CARTESIAN_POINT('Ctrl Pts',(7.63984896443366,0.0271238759470453,3.2943750240253));
#7617=CARTESIAN_POINT('Ctrl Pts',(7.58520989641712,0.232609561821433,3.33486742258247));
#7618=CARTESIAN_POINT('Ctrl Pts',(7.41956867650539,0.398792804467796,3.37952311993261));
#7619=CARTESIAN_POINT('Ctrl Pts',(7.1905457231359,0.460399855551445,3.42468394189214));
#7620=CARTESIAN_POINT('Ctrl Pts',(6.95869704927801,0.398681696943234,3.47035666953234));
#7621=CARTESIAN_POINT('Ctrl Pts',(6.78688141707536,0.227371623889039,3.51655404942707));
#7622=CARTESIAN_POINT('Ctrl Pts',(6.7229312949975,-0.00960578475399217,
3.5632735819084));
#7623=CARTESIAN_POINT('Ctrl Pts',(6.78694999671625,-0.249365465366649,3.61052175321115));
#7624=CARTESIAN_POINT('Ctrl Pts',(6.96406181917366,-0.427017015476016,3.65827815384324));
#7625=CARTESIAN_POINT('Ctrl Pts',(7.20884449734192,-0.492960246040882,3.70653567209578));
#7626=CARTESIAN_POINT('Ctrl Pts',(7.45620532585719,-0.427018438033829,3.75527364860311));
#7627=CARTESIAN_POINT('Ctrl Pts',(7.63922818507954,-0.244485987870997,3.80447044259358));
#7628=CARTESIAN_POINT('Ctrl Pts',(7.70120240491438,-0.0137441258516156,
3.84995779136607));
#7629=CARTESIAN_POINT('Ctrl Pts',(7.65913006311212,0.197656069537059,3.89160533681384));
#7630=CARTESIAN_POINT('Ctrl Pts',(7.55093165022181,0.359884525576526,3.9292907213808));
#7631=CARTESIAN_POINT('Ctrl Pts',(7.38795046396419,0.468807636689479,3.96717529387949));
#7632=CARTESIAN_POINT('Ctrl Pts',(7.19485944556467,0.507376335556598,4.00522949186857));
#7633=CARTESIAN_POINT('Ctrl Pts',(7.00092895437896,0.468801673803832,4.04343882565719));
#7634=CARTESIAN_POINT('Ctrl Pts',(6.83589776048967,0.358671322852951,4.08178585172935));
#7635=CARTESIAN_POINT('Ctrl Pts',(6.72525082625392,0.193231928470719,4.12024424860606));
#7636=CARTESIAN_POINT('Ctrl Pts',(6.68627533701788,-0.00244208003353348,
4.15880023983475));
#7637=CARTESIAN_POINT('Ctrl Pts',(6.72531069708358,-0.198468266862919,4.19742754656923));
#7638=CARTESIAN_POINT('Ctrl Pts',(6.83641060841933,-0.36494553097655,4.23610417128916));
#7639=CARTESIAN_POINT('Ctrl Pts',(7.00297752232982,-0.476160108331975,4.27480979854181));
#7640=CARTESIAN_POINT('Ctrl Pts',(7.19941745683392,-0.515336210269313,4.313521430379));
#7641=CARTESIAN_POINT('Ctrl Pts',(7.39577334638842,-0.476178009162295,4.35221655573581));
#7642=CARTESIAN_POINT('Ctrl Pts',(7.56210403701843,-0.365136489373791,4.39087303722902));
#7643=CARTESIAN_POINT('Ctrl Pts',(7.6729482105615,-0.198970065641914,4.42946934287203));
#7644=CARTESIAN_POINT('Ctrl Pts',(7.69886454791239,-0.0687900400044386,
4.45514378820058));
#7645=CARTESIAN_POINT('Ctrl Pts',(7.69887334379488,-0.003535760932353,4.46796371938795));
#7646=CARTESIAN_POINT('Ctrl Pts',(7.60521013505817,0.00687058616980481,
0.514997540570331));
#7647=CARTESIAN_POINT('Ctrl Pts',(7.60520291666221,0.0604213147496031,0.525518178609593));
#7648=CARTESIAN_POINT('Ctrl Pts',(7.58398553332829,0.167119405323871,0.546562317050415));
#7649=CARTESIAN_POINT('Ctrl Pts',(7.49271161354778,0.304100141680242,0.578374094337356));
#7650=CARTESIAN_POINT('Ctrl Pts',(7.35489249545306,0.396201765810716,0.610414265003916));
#7651=CARTESIAN_POINT('Ctrl Pts',(7.1910298751132,0.428986978304214,0.642713211662006));
#7652=CARTESIAN_POINT('Ctrl Pts',(7.02575974448701,0.396160852316168,0.675278092187565));
#7653=CARTESIAN_POINT('Ctrl Pts',(6.88431346091905,0.301887668071453,0.708126241652113));
#7654=CARTESIAN_POINT('Ctrl Pts',(6.78902288535122,0.159380649672213,0.741265999150335));
#7655=CARTESIAN_POINT('Ctrl Pts',(6.75495416610951,-0.0103780765937392,
0.774709380896621));
#7656=CARTESIAN_POINT('Ctrl Pts',(6.78918192236938,-0.181461258490112,0.808462327478204));
#7657=CARTESIAN_POINT('Ctrl Pts',(6.91885908336219,-0.377673922655746,0.853889424408574));
#7658=CARTESIAN_POINT('Ctrl Pts',(7.20977093093628,-0.499893892945984,0.911473809881342));
#7659=CARTESIAN_POINT('Ctrl Pts',(7.5072630858031,-0.377588681747576,0.97014125931953));
#7660=CARTESIAN_POINT('Ctrl Pts',(7.64330562270039,-0.172136868667308,1.01771468839021));
#7661=CARTESIAN_POINT('Ctrl Pts',(7.68999690574486,0.0575070029618808,1.06304113378557));
#7662=CARTESIAN_POINT('Ctrl Pts',(7.58912753114069,0.338304476334369,1.11835008292628));
#7663=CARTESIAN_POINT('Ctrl Pts',(7.28221724491026,0.515932878067702,1.18402351038321));
#7664=CARTESIAN_POINT('Ctrl Pts',(6.95856764177261,0.459622888930078,1.24500482688593));
#7665=CARTESIAN_POINT('Ctrl Pts',(6.75052714561547,0.251003536205887,1.30100630575919));
#7666=CARTESIAN_POINT('Ctrl Pts',(6.6812077153829,-0.00624875161643612,
1.35179871810002));
#7667=CARTESIAN_POINT('Ctrl Pts',(6.75038532199632,-0.2659051370397,1.40293663797005));
#7668=CARTESIAN_POINT('Ctrl Pts',(6.94135907381703,-0.45699229110439,1.45437635262256));
#7669=CARTESIAN_POINT('Ctrl Pts',(7.20350925771528,-0.527428674290956,1.50606241671445));
#7670=CARTESIAN_POINT('Ctrl Pts',(7.466748090342,-0.457001184800688,1.55794289327379));
#7671=CARTESIAN_POINT('Ctrl Pts',(7.65998094988944,-0.263878681039078,1.60996115190039));
#7672=CARTESIAN_POINT('Ctrl Pts',(7.73083750011286,0.000414812515617203,
1.66206037062288));
#7673=CARTESIAN_POINT('Ctrl Pts',(7.65998418428948,0.264828698515665,1.71418231635528));
#7674=CARTESIAN_POINT('Ctrl Pts',(7.46651390251919,0.458227587104288,1.76626886292904));
#7675=CARTESIAN_POINT('Ctrl Pts',(7.20273817979303,0.528826545134251,1.81826192542772));
#7676=CARTESIAN_POINT('Ctrl Pts',(6.93974476704769,0.45822214956276,1.87010491698065));
#7677=CARTESIAN_POINT('Ctrl Pts',(6.74813710185399,0.266377938570576,1.921741689797));
#7678=CARTESIAN_POINT('Ctrl Pts',(6.67836440043136,0.00561142794322326,
1.97312065809906));
#7679=CARTESIAN_POINT('Ctrl Pts',(6.73659880078668,-0.21008625780946,2.0156763602552));
#7680=CARTESIAN_POINT('Ctrl Pts',(6.84232372411288,-0.347442050898008,2.04954129133265));
#7681=CARTESIAN_POINT('Ctrl Pts',(6.9792275847297,-0.452713561295967,2.08327997196431));
#7682=CARTESIAN_POINT('Ctrl Pts',(7.19191177543547,-0.509527438177311,2.1252061938903));
#7683=CARTESIAN_POINT('Ctrl Pts',(7.44484173411992,-0.441538379734714,2.17507245803297));
#7684=CARTESIAN_POINT('Ctrl Pts',(7.62804734440532,-0.257793658448475,2.22446652563413));
#7685=CARTESIAN_POINT('Ctrl Pts',(7.68852622475162,-0.0303820434129393,
2.26927979174901));
#7686=CARTESIAN_POINT('Ctrl Pts',(7.64746376729105,0.174304350641336,2.30962934644072));
#7687=CARTESIAN_POINT('Ctrl Pts',(7.54392328379021,0.329181864553991,2.34563680278534));
#7688=CARTESIAN_POINT('Ctrl Pts',(7.39024341483315,0.431534873640089,2.38133009829314));
#7689=CARTESIAN_POINT('Ctrl Pts',(7.19076283221806,0.47124287783579,2.42063411117922));
#7690=CARTESIAN_POINT('Ctrl Pts',(6.97384163836222,0.412739485800526,2.46340945678261));
#7691=CARTESIAN_POINT('Ctrl Pts',(6.80305475944309,0.241271971337352,2.50949672429145));
#7692=CARTESIAN_POINT('Ctrl Pts',(6.74666636593271,0.0294294813802179,2.55121891282729));
#7693=CARTESIAN_POINT('Ctrl Pts',(6.78501449029175,-0.160618901754849,2.58873736232549));
#7694=CARTESIAN_POINT('Ctrl Pts',(6.91280587361007,-0.353262603670726,2.63334571969464));
#7695=CARTESIAN_POINT('Ctrl Pts',(7.19121233364888,-0.467932358310067,2.68834801025112));
#7696=CARTESIAN_POINT('Ctrl Pts',(7.51997563893116,-0.330454307712312,2.75322227387632));
#7697=CARTESIAN_POINT('Ctrl Pts',(7.63018823078828,-0.0608557124429638,
2.80643316177814));
#7698=CARTESIAN_POINT('Ctrl Pts',(7.58668367923284,0.15294955180044,2.84856125844144));
#7699=CARTESIAN_POINT('Ctrl Pts',(7.4966962551456,0.287961175664924,2.87995407749862));
#7700=CARTESIAN_POINT('Ctrl Pts',(7.36223523212543,0.377561342649274,2.91116449944352));
#7701=CARTESIAN_POINT('Ctrl Pts',(7.20471964510295,0.408886599560007,2.94221245706929));
#7702=CARTESIAN_POINT('Ctrl Pts',(7.04788050645387,0.377567269761301,2.97312030304224));
#7703=CARTESIAN_POINT('Ctrl Pts',(6.91541158632493,0.289068616916533,3.00391053762164));
#7704=CARTESIAN_POINT('Ctrl Pts',(6.82728400624535,0.156959448238268,3.03460541662168));
#7705=CARTESIAN_POINT('Ctrl Pts',(6.79284518780191,-0.0157081775009035,
3.06863471118277));
#7706=CARTESIAN_POINT('Ctrl Pts',(6.8434401979818,-0.205290308031978,3.10599536242566));
#7707=CARTESIAN_POINT('Ctrl Pts',(6.99490561515456,-0.356498560372845,3.14673092879048));
#7708=CARTESIAN_POINT('Ctrl Pts',(7.18440894248466,-0.407388834126994,3.18410164809681));
#7709=CARTESIAN_POINT('Ctrl Pts',(7.35718141101045,-0.372875605837951,3.2181429370676));
#7710=CARTESIAN_POINT('Ctrl Pts',(7.48936817162067,-0.284722401562679,3.24885612739662));
#7711=CARTESIAN_POINT('Ctrl Pts',(7.5779106915596,-0.152141452093539,3.27966780812697));
#7712=CARTESIAN_POINT('Ctrl Pts',(7.61281861301683,0.0222543255280253,3.31404069327135));
#7713=CARTESIAN_POINT('Ctrl Pts',(7.56141031644951,0.215151691836449,3.35205199924827));
#7714=CARTESIAN_POINT('Ctrl Pts',(7.40637132389603,0.370556257164557,3.39382812795649));
#7715=CARTESIAN_POINT('Ctrl Pts',(7.19266579688415,0.427969447901563,3.4359633441571));
#7716=CARTESIAN_POINT('Ctrl Pts',(6.97677320753052,0.370444592935496,3.47849574770186));
#7717=CARTESIAN_POINT('Ctrl Pts',(6.81697021686135,0.211073111139358,3.52146834643601));
#7718=CARTESIAN_POINT('Ctrl Pts',(6.7575107065363,-0.00928891171517924,
3.5649148319991));
#7719=CARTESIAN_POINT('Ctrl Pts',(6.8170432422483,-0.232336689376801,3.60886950546352));
#7720=CARTESIAN_POINT('Ctrl Pts',(6.98197068383346,-0.397821990347889,3.65335335844989));
#7721=CARTESIAN_POINT('Ctrl Pts',(7.21036126557627,-0.459413532859389,3.69838806473246));
#7722=CARTESIAN_POINT('Ctrl Pts',(7.44177728328924,-0.397805970847302,3.74398782560502));
#7723=CARTESIAN_POINT('Ctrl Pts',(7.61359761322389,-0.226593064877533,3.79016109241095));
#7724=CARTESIAN_POINT('Ctrl Pts',(7.67207491746036,-0.00928725692599748,
3.83301473789734));
#7725=CARTESIAN_POINT('Ctrl Pts',(7.63236648003885,0.190570754610721,3.87239027223786));
#7726=CARTESIAN_POINT('Ctrl Pts',(7.5297792392475,0.344489241168015,3.90814703559696));
#7727=CARTESIAN_POINT('Ctrl Pts',(7.37465784873898,0.448244015598285,3.94421635698774));
#7728=CARTESIAN_POINT('Ctrl Pts',(7.19013262440696,0.485169459790194,3.98059224783782));
#7729=CARTESIAN_POINT('Ctrl Pts',(7.00401824150362,0.448227922909911,4.01726483809911));
#7730=CARTESIAN_POINT('Ctrl Pts',(6.84494424822825,0.342162883311033,4.05422370431298));
#7731=CARTESIAN_POINT('Ctrl Pts',(6.7377790395693,0.182076193922272,4.09145704575414));
#7732=CARTESIAN_POINT('Ctrl Pts',(6.6998046109465,-0.00815538506850403,
4.12895008010636));
#7733=CARTESIAN_POINT('Ctrl Pts',(6.73784707742154,-0.199653661771381,4.16668775837162));
#7734=CARTESIAN_POINT('Ctrl Pts',(6.84681665964502,-0.363079625185603,4.20465459753528));
#7735=CARTESIAN_POINT('Ctrl Pts',(7.01102146739613,-0.472832785429877,4.24283021774106));
#7736=CARTESIAN_POINT('Ctrl Pts',(7.20565915814223,-0.511732666532225,4.28119783050688));
#7737=CARTESIAN_POINT('Ctrl Pts',(7.40119766392887,-0.472845697797204,4.31973380172215));
#7738=CARTESIAN_POINT('Ctrl Pts',(7.56768126051989,-0.361809343925003,4.358421783452));
#7739=CARTESIAN_POINT('Ctrl Pts',(7.67922282226515,-0.194826290524122,4.39723061348869));
#7740=CARTESIAN_POINT('Ctrl Pts',(7.70548232719575,-0.0632832490931723,
4.42318248066122));
#7741=CARTESIAN_POINT('Ctrl Pts',(7.70549122320354,0.00271383254598746,
4.43614834370058));
#7742=CARTESIAN_POINT('Ctrl Pts',(7.59425772000626,-0.00245828571258322,
0.562474587627441));
#7743=CARTESIAN_POINT('Ctrl Pts',(7.59425070209586,0.049605111382711,0.572703022803963));
#7744=CARTESIAN_POINT('Ctrl Pts',(7.57357837342717,0.153104623621763,0.593123233412961));
#7745=CARTESIAN_POINT('Ctrl Pts',(7.48570217383275,0.284704689582475,0.623707472840817));
#7746=CARTESIAN_POINT('Ctrl Pts',(7.35420545842841,0.372445934216777,0.654268165611503));
#7747=CARTESIAN_POINT('Ctrl Pts',(7.1991395427834,0.403344341615466,0.684830453955887));
#7748=CARTESIAN_POINT('Ctrl Pts',(7.04394708949579,0.372419394010662,0.715418389788155));
#7749=CARTESIAN_POINT('Ctrl Pts',(6.91208817981755,0.284411118321267,0.746056309925617));
#7750=CARTESIAN_POINT('Ctrl Pts',(6.82386012854329,0.15231772958913,0.776768674224976));
#7751=CARTESIAN_POINT('Ctrl Pts',(6.79256685119417,-0.00407665477365361,
0.80757840707805));
#7752=CARTESIAN_POINT('Ctrl Pts',(6.82398499489209,-0.160818309011226,0.838509649661102));
#7753=CARTESIAN_POINT('Ctrl Pts',(6.94235528076999,-0.339716384151892,0.879941146353341));
#7754=CARTESIAN_POINT('Ctrl Pts',(7.20619100564161,-0.450165980568156,0.932146935825043));
#7755=CARTESIAN_POINT('Ctrl Pts',(7.47426273580571,-0.339694216057503,0.985035363478316));
#7756=CARTESIAN_POINT('Ctrl Pts',(7.5966101933134,-0.154911117746058,1.02782858034605));
#7757=CARTESIAN_POINT('Ctrl Pts',(7.63856043476736,0.0514863727408663,1.0685660742741));
#7758=CARTESIAN_POINT('Ctrl Pts',(7.54796314564829,0.303787110641837,1.11826486854298));
#7759=CARTESIAN_POINT('Ctrl Pts',(7.27183799251809,0.463786696523768,1.17737021220891));
#7760=CARTESIAN_POINT('Ctrl Pts',(6.979509411796,0.413145867177907,1.23244288488132));
#7761=CARTESIAN_POINT('Ctrl Pts',(6.79065030465397,0.224010864274787,1.28324401250854));
#7762=CARTESIAN_POINT('Ctrl Pts',(6.72731021175071,-0.0104347042766862,
1.32953860130455));
#7763=CARTESIAN_POINT('Ctrl Pts',(6.79052629084231,-0.248473274721412,1.37640896854699));
#7764=CARTESIAN_POINT('Ctrl Pts',(6.96651190821311,-0.42488040938561,1.42384890860145));
#7765=CARTESIAN_POINT('Ctrl Pts',(7.20992736454157,-0.490534586687267,1.47184965533436));
#7766=CARTESIAN_POINT('Ctrl Pts',(7.45633551352294,-0.424884919868912,1.52039437044473));
#7767=CARTESIAN_POINT('Ctrl Pts',(7.63882761171195,-0.242897887840433,1.56946170079144));
#7768=CARTESIAN_POINT('Ctrl Pts',(7.70653270701263,0.00848210144412344,
1.61902445509968));
#7769=CARTESIAN_POINT('Ctrl Pts',(7.63882350593151,0.262379273284063,1.66905062455159));
#7770=CARTESIAN_POINT('Ctrl Pts',(7.45162606494433,0.449969447852711,1.71950325371943));
#7771=CARTESIAN_POINT('Ctrl Pts',(7.19376083718428,0.51933449850295,1.77034129362804));
#7772=CARTESIAN_POINT('Ctrl Pts',(6.93400990844331,0.449957716943267,1.82151919554189));
#7773=CARTESIAN_POINT('Ctrl Pts',(6.74275338990983,0.25894867906358,1.87298910713157));
#7774=CARTESIAN_POINT('Ctrl Pts',(6.6721794753372,-0.00344155851917735,
1.92469753383097));
#7775=CARTESIAN_POINT('Ctrl Pts',(6.7311016302344,-0.22275510874685,1.96794489965324));
#7776=CARTESIAN_POINT('Ctrl Pts',(6.8392913285343,-0.363404964177234,2.00260883790367));
#7777=CARTESIAN_POINT('Ctrl Pts',(6.98005366068073,-0.471713783449351,2.03730635823932));
#7778=CARTESIAN_POINT('Ctrl Pts',(7.20024838595684,-0.530815092622124,2.08071930878504));
#7779=CARTESIAN_POINT('Ctrl Pts',(7.4646816222063,-0.460071157751818,2.13283473795993));
#7780=CARTESIAN_POINT('Ctrl Pts',(7.65805360986435,-0.26656205273116,2.18490159146475));
#7781=CARTESIAN_POINT('Ctrl Pts',(7.72260468764345,-0.0248541589762378,
2.23253658214116));
#7782=CARTESIAN_POINT('Ctrl Pts',(7.67876439289767,0.194303019173836,2.27572981817065));
#7783=CARTESIAN_POINT('Ctrl Pts',(7.56739059632431,0.361091093887821,2.31449058128002));
#7784=CARTESIAN_POINT('Ctrl Pts',(7.40112190177162,0.471942442644023,2.3531164111895));
#7785=CARTESIAN_POINT('Ctrl Pts',(7.18420215947571,0.515230280020884,2.39586020388528));
#7786=CARTESIAN_POINT('Ctrl Pts',(6.94699552901196,0.451438689854431,2.4426223367052));
#7787=CARTESIAN_POINT('Ctrl Pts',(6.75916567417327,0.263096514005349,2.493274778268));
#7788=CARTESIAN_POINT('Ctrl Pts',(6.69679959781039,0.0292602423063323,2.53933073840707));
#7789=CARTESIAN_POINT('Ctrl Pts',(6.73922836906146,-0.181202753664555,2.5808764986312));
#7790=CARTESIAN_POINT('Ctrl Pts',(6.88098489158572,-0.395007257634639,2.6303774480251));
#7791=CARTESIAN_POINT('Ctrl Pts',(7.19061459426917,-0.522666325469509,2.69155654194586));
#7792=CARTESIAN_POINT('Ctrl Pts',(7.55656339289891,-0.369582360088882,2.76376828329337));
#7793=CARTESIAN_POINT('Ctrl Pts',(7.67882740451396,-0.0699592370443201,
2.8228934499334));
#7794=CARTESIAN_POINT('Ctrl Pts',(7.63057360286556,0.166780390817294,2.86954705222393));
#7795=CARTESIAN_POINT('Ctrl Pts',(7.53116289386047,0.315835424321569,2.90421442771358));
#7796=CARTESIAN_POINT('Ctrl Pts',(7.38316944888177,0.414366909131833,2.93855849946981));
#7797=CARTESIAN_POINT('Ctrl Pts',(7.21055140032512,0.448612501483557,2.97258326216516));
#7798=CARTESIAN_POINT('Ctrl Pts',(7.03953063478659,0.414371602633185,3.00629223766092));
#7799=CARTESIAN_POINT('Ctrl Pts',(6.89590035707824,0.318294406438298,3.03969251978853));
#7800=CARTESIAN_POINT('Ctrl Pts',(6.80097093648036,0.175798229922379,3.07279237357639));
#7801=CARTESIAN_POINT('Ctrl Pts',(6.76420446601918,-0.00918969341029978,
3.10924534420836));
#7802=CARTESIAN_POINT('Ctrl Pts',(6.81822428058444,-0.21055882798918,3.14894909070633));
#7803=CARTESIAN_POINT('Ctrl Pts',(6.97773218443497,-0.36935136486928,3.19179489876111));
#7804=CARTESIAN_POINT('Ctrl Pts',(7.17495518145593,-0.422006833075381,3.23067901466676));
#7805=CARTESIAN_POINT('Ctrl Pts',(7.35286337729078,-0.386309768778915,3.26574476462206));
#7806=CARTESIAN_POINT('Ctrl Pts',(7.48774464276126,-0.296188781696453,3.29710501689698));
#7807=CARTESIAN_POINT('Ctrl Pts',(7.57721901263156,-0.161961982729025,3.32828683420642));
#7808=CARTESIAN_POINT('Ctrl Pts',(7.61206314196752,0.0129508069889947,3.36275642269021));
#7809=CARTESIAN_POINT('Ctrl Pts',(7.56075482794487,0.204285379935896,3.40048407841003));
#7810=CARTESIAN_POINT('Ctrl Pts',(7.40850398946938,0.356408978558438,3.44145294697141));
#7811=CARTESIAN_POINT('Ctrl Pts',(7.20135390499387,0.41173394168823,3.48228578202979));
#7812=CARTESIAN_POINT('Ctrl Pts',(6.99457227847817,0.356315965170544,3.52304732856917));
#7813=CARTESIAN_POINT('Ctrl Pts',(6.84328577478245,0.205035111445078,3.56379125585673));
#7814=CARTESIAN_POINT('Ctrl Pts',(6.7877374954679,-0.00186586115036843,
3.60457861601043));
#7815=CARTESIAN_POINT('Ctrl Pts',(6.84333329257615,-0.209237336684351,3.64546113573529));
#7816=CARTESIAN_POINT('Ctrl Pts',(6.99562840241749,-0.361741579815771,3.68650281084151));
#7817=CARTESIAN_POINT('Ctrl Pts',(7.20485782405896,-0.417973379258145,3.72775549001309));
#7818=CARTESIAN_POINT('Ctrl Pts',(7.41548973555594,-0.361739190165172,3.76927272327787));
#7819=CARTESIAN_POINT('Ctrl Pts',(7.5710498247318,-0.206554713249447,3.81110431032449));
#7820=CARTESIAN_POINT('Ctrl Pts',(7.62374712773981,-0.0104230426211467,
3.84978234597979));
#7821=CARTESIAN_POINT('Ctrl Pts',(7.58796837467257,0.169522444365365,3.88523795926289));
#7822=CARTESIAN_POINT('Ctrl Pts',(7.49570620913085,0.307926121393348,3.91739357370391));
#7823=CARTESIAN_POINT('Ctrl Pts',(7.35630624460567,0.401161458520253,3.94980772489261));
#7824=CARTESIAN_POINT('Ctrl Pts',(7.19048793327558,0.434350296220375,3.98249611828477));
#7825=CARTESIAN_POINT('Ctrl Pts',(7.02313732463905,0.401152548579443,4.01547086689915));
#7826=CARTESIAN_POINT('Ctrl Pts',(6.87991827712017,0.305692036987412,4.04874191834322));
#7827=CARTESIAN_POINT('Ctrl Pts',(6.78324141246895,0.161344852331597,4.08231922585133));
#7828=CARTESIAN_POINT('Ctrl Pts',(6.74886677350852,-0.0105999920447858,
4.11620911872423));
#7829=CARTESIAN_POINT('Ctrl Pts',(6.78329499176258,-0.18420466099095,4.15041748648745));
#7830=CARTESIAN_POINT('Ctrl Pts',(6.88234563382671,-0.332882015591908,4.18494784070123));
#7831=CARTESIAN_POINT('Ctrl Pts',(7.03222479883265,-0.433150934079335,4.21980148929331));
#7832=CARTESIAN_POINT('Ctrl Pts',(7.21066650576015,-0.468899513976003,4.25497951717241));
#7833=CARTESIAN_POINT('Ctrl Pts',(7.39081341647505,-0.433166214217135,4.29047687728664));
#7834=CARTESIAN_POINT('Ctrl Pts',(7.54500124432846,-0.330435384103034,4.32629673150718));
#7835=CARTESIAN_POINT('Ctrl Pts',(7.648911736291,-0.175068311549345,4.36241691197868));
#7836=CARTESIAN_POINT('Ctrl Pts',(7.67356138220208,-0.051891031334385,4.38672007785258));
#7837=CARTESIAN_POINT('Ctrl Pts',(7.67356972993859,0.010038573569273,4.39888683970507));
#7838=CARTESIAN_POINT('Ctrl Pts',(7.6251463906065,-0.00995933879406772,
0.600676626589758));
#7839=CARTESIAN_POINT('Ctrl Pts',(7.62513886057627,0.0459032942528346,0.611651464053095));
#7840=CARTESIAN_POINT('Ctrl Pts',(7.60292290623068,0.156870790432269,0.633544848495396));
#7841=CARTESIAN_POINT('Ctrl Pts',(7.50931870776666,0.296831365590117,0.666081330908944));
#7842=CARTESIAN_POINT('Ctrl Pts',(7.37036934701443,0.389419470623286,0.698359968830145));
#7843=CARTESIAN_POINT('Ctrl Pts',(7.20784862587356,0.421674331381802,0.730381922456915));
#7844=CARTESIAN_POINT('Ctrl Pts',(7.04659254578026,0.389405737732574,0.762169124409136));
#7845=CARTESIAN_POINT('Ctrl Pts',(6.91079445014922,0.298603087234844,0.793736135243985));
#7846=CARTESIAN_POINT('Ctrl Pts',(6.8207979343427,0.163604010555256,0.825103242993061));
#7847=CARTESIAN_POINT('Ctrl Pts',(6.78926618396683,0.00524540576184069,
0.856289595657219));
#7848=CARTESIAN_POINT('Ctrl Pts',(6.82091005115504,-0.151956334869631,0.887316325014752));
#7849=CARTESIAN_POINT('Ctrl Pts',(6.93880442644738,-0.329744857889583,0.928502477696562));
#7850=CARTESIAN_POINT('Ctrl Pts',(7.19794632806152,-0.437170841618844,0.97969295172908));
#7851=CARTESIAN_POINT('Ctrl Pts',(7.45594932305352,-0.329838555678054,1.03065941290864));
#7852=CARTESIAN_POINT('Ctrl Pts',(7.57223630638577,-0.15388196293264,1.07139312359183));
#7853=CARTESIAN_POINT('Ctrl Pts',(7.61173195193373,0.0411613828711062,1.10987247621873));
#7854=CARTESIAN_POINT('Ctrl Pts',(7.52649198341673,0.276889962424743,1.15632864381613));
#7855=CARTESIAN_POINT('Ctrl Pts',(7.27100861906712,0.424277981015224,1.21095498218268));
#7856=CARTESIAN_POINT('Ctrl Pts',(7.00347558016671,0.377525264901119,1.26136760852975));
#7857=CARTESIAN_POINT('Ctrl Pts',(6.83192597243994,0.205463838889712,1.30754770952591));
#7858=CARTESIAN_POINT('Ctrl Pts',(6.77471877393629,-0.00671405179287721,
1.34943621263325));
#7859=CARTESIAN_POINT('Ctrl Pts',(6.83181225604176,-0.221332534887357,1.39169859189476));
#7860=CARTESIAN_POINT('Ctrl Pts',(6.99015954735038,-0.379977992431842,1.43437163868664));
#7861=CARTESIAN_POINT('Ctrl Pts',(7.20886960086134,-0.438945066985825,1.47749887936028));
#7862=CARTESIAN_POINT('Ctrl Pts',(7.43024747996125,-0.379973659956208,1.52111182668763));
#7863=CARTESIAN_POINT('Ctrl Pts',(7.59439894652586,-0.216337713478778,1.56524030048575));
#7864=CARTESIAN_POINT('Ctrl Pts',(7.65548722497565,0.0101858356141963,1.60990738944098));
#7865=CARTESIAN_POINT('Ctrl Pts',(7.59438357985085,0.239727786394584,1.65513131383826));
#7866=CARTESIAN_POINT('Ctrl Pts',(7.42458127262742,0.410079670414055,1.70092433297305));
#7867=CARTESIAN_POINT('Ctrl Pts',(7.1894457064806,0.473501570956881,1.74729294719369));
#7868=CARTESIAN_POINT('Ctrl Pts',(6.95114935036374,0.410054983182796,1.79423785660882));
#7869=CARTESIAN_POINT('Ctrl Pts',(6.77444906673486,0.233888130858127,1.8417535579876));
#7870=CARTESIAN_POINT('Ctrl Pts',(6.70860511145662,-0.00997119589789413,
1.8898294385356));
#7871=CARTESIAN_POINT('Ctrl Pts',(6.76359263836854,-0.215478331596112,1.93034449371185));
#7872=CARTESIAN_POINT('Ctrl Pts',(6.86552920528386,-0.348073042081005,1.96301641877778));
#7873=CARTESIAN_POINT('Ctrl Pts',(6.99871512481987,-0.450608012381444,1.99585725873467));
#7874=CARTESIAN_POINT('Ctrl Pts',(7.20840141309144,-0.50713987259909,2.03721833824704));
#7875=CARTESIAN_POINT('Ctrl Pts',(7.46261403294825,-0.439449176754183,2.08730887227053));
#7876=CARTESIAN_POINT('Ctrl Pts',(7.65043036508478,-0.251969993404681,2.13782457411003));
#7877=CARTESIAN_POINT('Ctrl Pts',(7.71393504862941,-0.0153445846184741,
2.1844803492873));
#7878=CARTESIAN_POINT('Ctrl Pts',(7.67080165909933,0.201106000343718,2.22713471421714));
#7879=CARTESIAN_POINT('Ctrl Pts',(7.56014087497921,0.367078706762164,2.2656927101989));
#7880=CARTESIAN_POINT('Ctrl Pts',(7.39362722575602,0.47826661439383,2.30439640224526));
#7881=CARTESIAN_POINT('Ctrl Pts',(7.17474883695495,0.5221088112285,2.34753793394624));
#7882=CARTESIAN_POINT('Ctrl Pts',(6.93323485822253,0.457485550857918,2.39514037933818));
#7883=CARTESIAN_POINT('Ctrl Pts',(6.73999704643146,0.264200773821966,2.44718908940685));
#7884=CARTESIAN_POINT('Ctrl Pts',(6.6750106891604,0.0217479615274458,2.49496582442984));
#7885=CARTESIAN_POINT('Ctrl Pts',(6.71923769435572,-0.198307386666359,2.53840100430929));
#7886=CARTESIAN_POINT('Ctrl Pts',(6.86820572152663,-0.423361666552716,2.59049654373951));
#7887=CARTESIAN_POINT('Ctrl Pts',(7.19683451438197,-0.559762287000885,2.65550316184341));
#7888=CARTESIAN_POINT('Ctrl Pts',(7.59061985625878,-0.39609337580252,2.73313735372284));
#7889=CARTESIAN_POINT('Ctrl Pts',(7.72404765466645,-0.0708376341742968,
2.79737041159043));
#7890=CARTESIAN_POINT('Ctrl Pts',(7.67138895603303,0.188103473826818,2.84838979927756));
#7891=CARTESIAN_POINT('Ctrl Pts',(7.56230591732181,0.35178346601004,2.88645331216893));
#7892=CARTESIAN_POINT('Ctrl Pts',(7.39927679222285,0.46041116731156,2.92429660886102));
#7893=CARTESIAN_POINT('Ctrl Pts',(7.2085057862945,0.498313460595825,2.96190202559112));
#7894=CARTESIAN_POINT('Ctrl Pts',(7.01899650553946,0.460419063486977,2.99925417953252));
#7895=CARTESIAN_POINT('Ctrl Pts',(6.8595074148951,0.353776728734024,3.03633740791343));
#7896=CARTESIAN_POINT('Ctrl Pts',(6.75393754656612,0.195352351115091,3.07314022143174));
#7897=CARTESIAN_POINT('Ctrl Pts',(6.71300839906166,-0.0105024876967131,
3.11370534962017));
#7898=CARTESIAN_POINT('Ctrl Pts',(6.77313540889629,-0.23465187277845,3.1578981321776));
#7899=CARTESIAN_POINT('Ctrl Pts',(6.9505773913537,-0.411233490999672,3.2055512312233));
#7900=CARTESIAN_POINT('Ctrl Pts',(7.16952277235119,-0.469618095917656,3.24871160420247));
#7901=CARTESIAN_POINT('Ctrl Pts',(7.36645966236824,-0.430046136418131,3.28752910700568));
#7902=CARTESIAN_POINT('Ctrl Pts',(7.51530337347556,-0.330531283613474,3.322140113292));
#7903=CARTESIAN_POINT('Ctrl Pts',(7.6136393067511,-0.182885406541807,3.35642864300427));
#7904=CARTESIAN_POINT('Ctrl Pts',(7.6517119731009,0.00866863156965702,3.39417116601774));
#7905=CARTESIAN_POINT('Ctrl Pts',(7.59566292791954,0.216926348779987,3.43523841335543));
#7906=CARTESIAN_POINT('Ctrl Pts',(7.43098841093127,0.381112304766534,3.47949475317577));
#7907=CARTESIAN_POINT('Ctrl Pts',(7.20902257822881,0.440109346407386,3.52323182285004));
#7908=CARTESIAN_POINT('Ctrl Pts',(6.98969677272196,0.381025501634275,3.56647300951898));
#7909=CARTESIAN_POINT('Ctrl Pts',(6.83104480220145,0.221934930884199,3.60925399866409));
#7910=CARTESIAN_POINT('Ctrl Pts',(6.77366702945068,0.00694265778365469,
3.6516094283646));
#7911=CARTESIAN_POINT('Ctrl Pts',(6.8310824464219,-0.205902622087142,3.6935863577146));
#7912=CARTESIAN_POINT('Ctrl Pts',(6.98586160732495,-0.360410071323003,3.73522365094446));
#7913=CARTESIAN_POINT('Ctrl Pts',(7.19571361575979,-0.416451275528931,3.77657387332006));
#7914=CARTESIAN_POINT('Ctrl Pts',(7.40425474387956,-0.360423855799516,3.81768805486677));
#7915=CARTESIAN_POINT('Ctrl Pts',(7.5562630491962,-0.208304194865644,3.85862159368099));
#7916=CARTESIAN_POINT('Ctrl Pts',(7.60695606004407,-0.0185100802651633,
3.89602785586108));
#7917=CARTESIAN_POINT('Ctrl Pts',(7.57254113144743,0.153827290746397,3.92998748438201));
#7918=CARTESIAN_POINT('Ctrl Pts',(7.48477263414739,0.28527139080477,3.96053536270553));
#7919=CARTESIAN_POINT('Ctrl Pts',(7.35326159780128,0.373088001773748,3.99109827766809));
#7920=CARTESIAN_POINT('Ctrl Pts',(7.19801139434241,0.404051485210006,4.02169520823128));
#7921=CARTESIAN_POINT('Ctrl Pts',(7.04242854792053,0.373082428795767,4.05235230289711));
#7922=CARTESIAN_POINT('Ctrl Pts',(6.91013509296653,0.284793306662795,4.08309464265432));
#7923=CARTESIAN_POINT('Ctrl Pts',(6.82137789485868,0.152112705303776,4.11394287723527));
#7924=CARTESIAN_POINT('Ctrl Pts',(6.79002667088262,-0.00509640153436752,
4.14492325438676));
#7925=CARTESIAN_POINT('Ctrl Pts',(6.82142807903689,-0.163089310650938,4.17605557225883));
#7926=CARTESIAN_POINT('Ctrl Pts',(6.9112855133859,-0.297866472185936,4.20736152086343));
#7927=CARTESIAN_POINT('Ctrl Pts',(7.04678082670187,-0.388454515500582,4.23886139687883));
#7928=CARTESIAN_POINT('Ctrl Pts',(7.20767263671213,-0.420652573613419,4.27057542931576));
#7929=CARTESIAN_POINT('Ctrl Pts',(7.36979084225692,-0.388467264966068,4.30251884135981));
#7930=CARTESIAN_POINT('Ctrl Pts',(7.50837984637881,-0.296115525357199,4.3347137808459));
#7931=CARTESIAN_POINT('Ctrl Pts',(7.60172624083291,-0.156526571753314,4.36716218083725));
#7932=CARTESIAN_POINT('Ctrl Pts',(7.62387694790615,-0.0458686559730776,
4.38899381459629));
#7933=CARTESIAN_POINT('Ctrl Pts',(7.62388445692499,0.00983872883570376,
4.39993815188776));
#7934=CARTESIAN_POINT('Ctrl Pts',(7.67479866661154,-0.00992467619824002,
0.600534259038771));
#7935=CARTESIAN_POINT('Ctrl Pts',(7.67479029797541,0.0521592777126054,0.612731344390634));
#7936=CARTESIAN_POINT('Ctrl Pts',(7.6500767264732,0.175648933321932,0.637096797205508));
#7937=CARTESIAN_POINT('Ctrl Pts',(7.54588794825347,0.331423934572361,0.673313288688549));
#7938=CARTESIAN_POINT('Ctrl Pts',(7.39127793836307,0.434435241125366,0.709231481896876));
#7939=CARTESIAN_POINT('Ctrl Pts',(7.21062039986564,0.470261715425624,0.744828861653363));
#7940=CARTESIAN_POINT('Ctrl Pts',(7.03167221168909,0.434417722011693,0.780107884329232));
#7941=CARTESIAN_POINT('Ctrl Pts',(6.88134081087794,0.333835280809163,0.815063046988659));
#7942=CARTESIAN_POINT('Ctrl Pts',(6.78203321069345,0.184769764667609,0.849694716646961));
#7943=CARTESIAN_POINT('Ctrl Pts',(6.74742301017565,0.0105515865458462,0.884003789334016));
#7944=CARTESIAN_POINT('Ctrl Pts',(6.7821506919055,-0.161614361391387,0.917993137651611));
#7945=CARTESIAN_POINT('Ctrl Pts',(6.91079450905087,-0.35538315192201,0.962892520561796));
#7946=CARTESIAN_POINT('Ctrl Pts',(7.19125186153526,-0.470870066280229,1.01824785147389));
#7947=CARTESIAN_POINT('Ctrl Pts',(7.46622186533978,-0.355583864325095,1.07263464146893));
#7948=CARTESIAN_POINT('Ctrl Pts',(7.58869616833744,-0.169899793625554,1.11561531576428));
#7949=CARTESIAN_POINT('Ctrl Pts',(7.62989084686889,0.0343026557437226,1.1558927821855));
#7950=CARTESIAN_POINT('Ctrl Pts',(7.54102211851986,0.278002087645062,1.20397798366483));
#7951=CARTESIAN_POINT('Ctrl Pts',(7.28038899375006,0.427368120216494,1.25963095207772));
#7952=CARTESIAN_POINT('Ctrl Pts',(7.01236273858795,0.379779461323442,1.31016266895165));
#7953=CARTESIAN_POINT('Ctrl Pts',(6.84312930177798,0.209454684258967,1.35581730583755));
#7954=CARTESIAN_POINT('Ctrl Pts',(6.7875566642785,0.00215073089889336,1.39673552660572));
#7955=CARTESIAN_POINT('Ctrl Pts',(6.84299249099257,-0.204955992335496,1.43753752961745));
#7956=CARTESIAN_POINT('Ctrl Pts',(6.99438077830621,-0.356203083369992,1.47828922226758));
#7957=CARTESIAN_POINT('Ctrl Pts',(7.20108707217728,-0.411642052898573,1.51904138345725));
#7958=CARTESIAN_POINT('Ctrl Pts',(7.40815060417183,-0.356215475951744,1.55985546395848));
#7959=CARTESIAN_POINT('Ctrl Pts',(7.56022255433633,-0.204292849888386,1.6007875102571));
#7960=CARTESIAN_POINT('Ctrl Pts',(7.6162350845383,0.00419615192836477,1.64189449134062));
#7961=CARTESIAN_POINT('Ctrl Pts',(7.56022316647258,0.213929952633467,1.68323060525625));
#7962=CARTESIAN_POINT('Ctrl Pts',(7.40582151724235,0.368627873830385,1.72484818318265));
#7963=CARTESIAN_POINT('Ctrl Pts',(7.19309620708298,0.42588980315725,1.7667963623234));
#7964=CARTESIAN_POINT('Ctrl Pts',(6.97829166980193,0.368617545064421,1.80912125797898));
#7965=CARTESIAN_POINT('Ctrl Pts',(6.81938158401184,0.210124736402539,1.85186448361653));
#7966=CARTESIAN_POINT('Ctrl Pts',(6.76022871604125,-0.00899134529255971,
1.89506476553187));
#7967=CARTESIAN_POINT('Ctrl Pts',(6.80961939806014,-0.193661886224269,1.93147173029523));
#7968=CARTESIAN_POINT('Ctrl Pts',(6.90128880494812,-0.312919191995625,1.96085533209598));
#7969=CARTESIAN_POINT('Ctrl Pts',(7.02116296768677,-0.405217714775714,1.99041541019261));
#7970=CARTESIAN_POINT('Ctrl Pts',(7.2101902287687,-0.456256683551471,2.0277044964254));
#7971=CARTESIAN_POINT('Ctrl Pts',(7.44013817723507,-0.39514737391709,2.07300715398026));
#7972=CARTESIAN_POINT('Ctrl Pts',(7.61080888298339,-0.224999902344798,2.11888000691673));
#7973=CARTESIAN_POINT('Ctrl Pts',(7.66892725315019,-0.00908328955551635,
2.16145591840512));
#7974=CARTESIAN_POINT('Ctrl Pts',(7.62945122739719,0.189485836845824,2.20058130338214));
#7975=CARTESIAN_POINT('Ctrl Pts',(7.5275438271907,0.342497311992806,2.23611409854177));
#7976=CARTESIAN_POINT('Ctrl Pts',(7.37334783976495,0.445576027600189,2.27196416979245));
#7977=CARTESIAN_POINT('Ctrl Pts',(7.16952106168795,0.486525787486152,2.31214252862709));
#7978=CARTESIAN_POINT('Ctrl Pts',(6.94300344132289,0.42617239887457,2.35676948181569));
#7979=CARTESIAN_POINT('Ctrl Pts',(6.76011882687655,0.243647090636264,2.40597173678973));
#7980=CARTESIAN_POINT('Ctrl Pts',(6.69787591763812,0.0125389329026939,2.45151668259076));
#7981=CARTESIAN_POINT('Ctrl Pts',(6.74025578358462,-0.198992447969517,2.49325466511179));
#7982=CARTESIAN_POINT('Ctrl Pts',(6.88420849211811,-0.41683400693851,2.54365885019681));
#7983=CARTESIAN_POINT('Ctrl Pts',(7.20519838849559,-0.551093588719466,2.60722003202361));
#7984=CARTESIAN_POINT('Ctrl Pts',(7.59637091882833,-0.389875109666415,2.68423239344864));
#7985=CARTESIAN_POINT('Ctrl Pts',(7.73161202088386,-0.0627950541721369,
2.74887995748231));
#7986=CARTESIAN_POINT('Ctrl Pts',(7.67821621404377,0.200815500874292,2.800795072092));
#7987=CARTESIAN_POINT('Ctrl Pts',(7.56652799154434,0.368635913177726,2.8398029009376));
#7988=CARTESIAN_POINT('Ctrl Pts',(7.39832631725958,0.480881956369855,2.87885956424108));
#7989=CARTESIAN_POINT('Ctrl Pts',(7.20007842418665,0.520408671552025,2.91794004656954));
#7990=CARTESIAN_POINT('Ctrl Pts',(7.00175111169393,0.48088156284492,2.95701986564842));
#7991=CARTESIAN_POINT('Ctrl Pts',(6.83369430575371,0.368667574968921,2.99607525105644));
#7992=CARTESIAN_POINT('Ctrl Pts',(6.72169316671637,0.200802407429077,3.03507982827121));
#7993=CARTESIAN_POINT('Ctrl Pts',(6.6779145850631,-0.0187059625261386,3.0783398943622));
#7994=CARTESIAN_POINT('Ctrl Pts',(6.74223823189394,-0.259425539513033,3.12578113707604));
#7995=CARTESIAN_POINT('Ctrl Pts',(6.93397723224707,-0.450570898703853,3.17731127091177));
#7996=CARTESIAN_POINT('Ctrl Pts',(7.1722647119663,-0.51431424077328,3.22429041505122));
#7997=CARTESIAN_POINT('Ctrl Pts',(7.38777183560922,-0.471096886879066,3.26675960479394));
#7998=CARTESIAN_POINT('Ctrl Pts',(7.55131219363285,-0.361840084601825,3.30477820464692));
#7999=CARTESIAN_POINT('Ctrl Pts',(7.65975942831194,-0.199115335498351,3.34257273329541));
#8000=CARTESIAN_POINT('Ctrl Pts',(7.70191108793092,0.0126587082651895,3.38430173234848));
#8001=CARTESIAN_POINT('Ctrl Pts',(7.63984171392963,0.24359688777398,3.42983440925146));
#8002=CARTESIAN_POINT('Ctrl Pts',(7.45686243056377,0.426111652973154,3.47901961565964));
#8003=CARTESIAN_POINT('Ctrl Pts',(7.20986017068608,0.491783017499628,3.52768953921784));
#8004=CARTESIAN_POINT('Ctrl Pts',(6.96574932197927,0.42600252056967,3.57581950032201));
#8005=CARTESIAN_POINT('Ctrl Pts',(6.78936748485555,0.249056980614626,3.62339237126234));
#8006=CARTESIAN_POINT('Ctrl Pts',(6.72578712981547,0.0104579783117708,3.6703970656946));
#8007=CARTESIAN_POINT('Ctrl Pts',(6.78941191873306,-0.22492423847484,3.71682678335395));
#8008=CARTESIAN_POINT('Ctrl Pts',(6.9599707009394,-0.394951542887189,3.76268295455715));
#8009=CARTESIAN_POINT('Ctrl Pts',(7.18982623952553,-0.456130340124368,3.80797027228821));
#8010=CARTESIAN_POINT('Ctrl Pts',(7.41661698388298,-0.394964306963868,3.8527010569297));
#8011=CARTESIAN_POINT('Ctrl Pts',(7.58051422722045,-0.230580202674474,3.89689197253134));
#8012=CARTESIAN_POINT('Ctrl Pts',(7.63450803247875,-0.0274292607074651,
3.9369279396462));
#8013=CARTESIAN_POINT('Ctrl Pts',(7.59785383835248,0.155398772912859,3.97296600933491));
#8014=CARTESIAN_POINT('Ctrl Pts',(7.50532059797367,0.293739897374131,4.00514140052698));
#8015=CARTESIAN_POINT('Ctrl Pts',(7.36788217274004,0.385354559507254,4.03706791208184));
#8016=CARTESIAN_POINT('Ctrl Pts',(7.2070357335576,0.417288319469129,4.06876724211276));
#8017=CARTESIAN_POINT('Ctrl Pts',(7.04729419715336,0.385346151743235,4.10025531214439));
#8018=CARTESIAN_POINT('Ctrl Pts',(6.9127169339232,0.295357215095775,4.13155072863576));
#8019=CARTESIAN_POINT('Ctrl Pts',(6.8233007999502,0.16142663300187,4.16267626015357));
#8020=CARTESIAN_POINT('Ctrl Pts',(6.79210610834504,0.00424230951374864,
4.19365003347802));
#8021=CARTESIAN_POINT('Ctrl Pts',(6.82335152241767,-0.152245393365304,4.22449627052708));
#8022=CARTESIAN_POINT('Ctrl Pts',(6.91170118225541,-0.284497538555319,4.2552382224001));
#8023=CARTESIAN_POINT('Ctrl Pts',(7.0436328417148,-0.372545139247727,4.28589810740223));
#8024=CARTESIAN_POINT('Ctrl Pts',(7.19889934274857,-0.403485302426958,4.31650036598566));
#8025=CARTESIAN_POINT('Ctrl Pts',(7.35398823305083,-0.372573048928812,4.34706944683436));
#8026=CARTESIAN_POINT('Ctrl Pts',(7.48547509251604,-0.284834315514199,4.37762904432927));
#8027=CARTESIAN_POINT('Ctrl Pts',(7.57331921955373,-0.153270744978136,4.4082049409292));
#8028=CARTESIAN_POINT('Ctrl Pts',(7.59397776075199,-0.0498297474199503,
4.42861399797485));
#8029=CARTESIAN_POINT('Ctrl Pts',(7.59398477416145,0.00220084515175098,
4.43883598840815));
#8030=CARTESIAN_POINT('Ctrl Pts',(7.70589891767588,-0.00245359116008025,
0.562527291052974));
#8031=CARTESIAN_POINT('Ctrl Pts',(7.70589001475021,0.0635940679486153,0.57550309050989));
#8032=CARTESIAN_POINT('Ctrl Pts',(7.67960751727991,0.195246334704192,0.601476943597424));
#8033=CARTESIAN_POINT('Ctrl Pts',(7.56794704817328,0.362402774430045,0.640326865453731));
#8034=CARTESIAN_POINT('Ctrl Pts',(7.40125695808951,0.473579993253837,0.679063145032516));
#8035=CARTESIAN_POINT('Ctrl Pts',(7.20543306486306,0.512518883001897,0.71765425115707));
#8036=CARTESIAN_POINT('Ctrl Pts',(7.01048476585089,0.47356858176727,0.75608392728287));
#8037=CARTESIAN_POINT('Ctrl Pts',(6.84596393699636,0.363597944823763,0.794327562675024));
#8038=CARTESIAN_POINT('Ctrl Pts',(6.73681549467478,0.199907515410705,0.832368570550477));
#8039=CARTESIAN_POINT('Ctrl Pts',(6.69859516683231,0.00788873917180853,
0.870185654844328));
#8040=CARTESIAN_POINT('Ctrl Pts',(6.73693840908256,-0.182462612245687,0.907764070762306));
#8041=CARTESIAN_POINT('Ctrl Pts',(6.87944326222088,-0.397259890598946,0.957526324120129));
#8042=CARTESIAN_POINT('Ctrl Pts',(7.19112164610969,-0.52580429954268,1.019055817578));
#8043=CARTESIAN_POINT('Ctrl Pts',(7.49727265912014,-0.397485516076704,1.07960188006838));
#8044=CARTESIAN_POINT('Ctrl Pts',(7.63350319008322,-0.190883659121824,1.12741548650668));
#8045=CARTESIAN_POINT('Ctrl Pts',(7.67926654816378,0.0360593370384181,1.17217372176293));
#8046=CARTESIAN_POINT('Ctrl Pts',(7.58056509985602,0.306162895092056,1.2254647678339));
#8047=CARTESIAN_POINT('Ctrl Pts',(7.29294272175984,0.470562172818316,1.28683106259674));
#8048=CARTESIAN_POINT('Ctrl Pts',(6.99954581718474,0.418054042402384,1.34215587872395));
#8049=CARTESIAN_POINT('Ctrl Pts',(6.81596154951457,0.232892123969687,1.39172465766909));
#8050=CARTESIAN_POINT('Ctrl Pts',(6.75631856140084,0.00947775492955636,
1.43580133529387));
#8051=CARTESIAN_POINT('Ctrl Pts',(6.8157947547332,-0.211634317055903,1.4793685868871));
#8052=CARTESIAN_POINT('Ctrl Pts',(6.97609023807819,-0.371345558222595,1.52244706084194));
#8053=CARTESIAN_POINT('Ctrl Pts',(7.1924649342669,-0.429050195429467,1.56507891751011));
#8054=CARTESIAN_POINT('Ctrl Pts',(7.4066375984947,-0.37137171946741,1.6072994439806));
#8055=CARTESIAN_POINT('Ctrl Pts',(7.56193269569475,-0.215745610884436,1.64915326420547));
#8056=CARTESIAN_POINT('Ctrl Pts',(7.61820626718149,-0.00494726647780665,
1.69068645168105));
#8057=CARTESIAN_POINT('Ctrl Pts',(7.561944028498,0.204380228806823,1.7319494515681));
#8058=CARTESIAN_POINT('Ctrl Pts',(7.40938473246838,0.356749091593267,1.77299486946184));
#8059=CARTESIAN_POINT('Ctrl Pts',(7.20192341170518,0.41224876158547,1.81387806697088));
#8060=CARTESIAN_POINT('Ctrl Pts',(6.99500876965101,0.35674779749565,1.85465522832279));
#8061=CARTESIAN_POINT('Ctrl Pts',(6.84376585084722,0.205473612051122,1.89538529487664));
#8062=CARTESIAN_POINT('Ctrl Pts',(6.78825237597385,-0.00128361409126172,
1.93612397126094));
#8063=CARTESIAN_POINT('Ctrl Pts',(6.83460167043985,-0.173751988890528,1.97013317734193));
#8064=CARTESIAN_POINT('Ctrl Pts',(6.91971539174711,-0.284417737520675,1.99740528786609));
#8065=CARTESIAN_POINT('Ctrl Pts',(7.030558325938,-0.369712270987243,2.02472860539297));
#8066=CARTESIAN_POINT('Ctrl Pts',(7.20432462750735,-0.416450035553709,2.05899164095769));
#8067=CARTESIAN_POINT('Ctrl Pts',(7.41421871524057,-0.360487797716962,2.10035061982331));
#8068=CARTESIAN_POINT('Ctrl Pts',(7.56905709734982,-0.20590418677377,2.14199286175633));
#8069=CARTESIAN_POINT('Ctrl Pts',(7.62148773641759,-0.0107077758477395,
2.1804754775963));
#8070=CARTESIAN_POINT('Ctrl Pts',(7.58586473971553,0.168272748684638,2.215741820189));
#8071=CARTESIAN_POINT('Ctrl Pts',(7.49414435933883,0.305939339339139,2.2477146319058));
#8072=CARTESIAN_POINT('Ctrl Pts',(7.35554181248979,0.398575104482043,2.27993674611506));
#8073=CARTESIAN_POINT('Ctrl Pts',(7.1724244687894,0.435355812617659,2.31603381922843));
#8074=CARTESIAN_POINT('Ctrl Pts',(6.96887901773368,0.381138200319487,2.35613647030697));
#8075=CARTESIAN_POINT('Ctrl Pts',(6.80429530787655,0.216951871529364,2.40040714688527));
#8076=CARTESIAN_POINT('Ctrl Pts',(6.74808716941278,0.00854379166712036,
2.44148821315331));
#8077=CARTESIAN_POINT('Ctrl Pts',(6.78637616860293,-0.182801008849154,2.47924298930385));
#8078=CARTESIAN_POINT('Ctrl Pts',(6.91689579762816,-0.380440663799344,2.52497536795987));
#8079=CARTESIAN_POINT('Ctrl Pts',(7.20943026727739,-0.503307468048506,2.58295046852016));
#8080=CARTESIAN_POINT('Ctrl Pts',(7.56960218122422,-0.355688097435077,2.65381590527583));
#8081=CARTESIAN_POINT('Ctrl Pts',(7.69596854078112,-0.0518610909867873,
2.71393040986061));
#8082=CARTESIAN_POINT('Ctrl Pts',(7.64605614650999,0.195429699182056,2.7626228521922));
#8083=CARTESIAN_POINT('Ctrl Pts',(7.54075491725149,0.353823956190948,2.79943586318946));
#8084=CARTESIAN_POINT('Ctrl Pts',(7.38110265703664,0.460523419655934,2.83652916749481));
#8085=CARTESIAN_POINT('Ctrl Pts',(7.19162995349104,0.498419629258629,2.8738910248991));
#8086=CARTESIAN_POINT('Ctrl Pts',(7.0007409604579,0.460513246952508,2.91150596794594));
#8087=CARTESIAN_POINT('Ctrl Pts',(6.8378190554252,0.35188377722391,2.94935771811315));
#8088=CARTESIAN_POINT('Ctrl Pts',(6.72839911208997,0.188136424398707,2.98743075002918));
#8089=CARTESIAN_POINT('Ctrl Pts',(6.6852206077216,-0.027573090972768,3.02995304677867));
#8090=CARTESIAN_POINT('Ctrl Pts',(6.74868061440645,-0.266253983865906,3.07699473012916));
#8091=CARTESIAN_POINT('Ctrl Pts',(6.94034313197966,-0.457833475149794,3.12857952778403));
#8092=CARTESIAN_POINT('Ctrl Pts',(7.18108231512846,-0.522550362879875,3.17606797384646));
#8093=CARTESIAN_POINT('Ctrl Pts',(7.40075884064422,-0.478672810860648,3.21935714251314));
#8094=CARTESIAN_POINT('Ctrl Pts',(7.56869285653519,-0.36664527074508,3.25838491270649));
#8095=CARTESIAN_POINT('Ctrl Pts',(7.6809146021808,-0.198518993827375,3.29745824706686));
#8096=CARTESIAN_POINT('Ctrl Pts',(7.72493145536016,0.0218557872720809,3.34089199698168));
#8097=CARTESIAN_POINT('Ctrl Pts',(7.66010664182934,0.264194720858232,3.38867061296822));
#8098=CARTESIAN_POINT('Ctrl Pts',(7.46671346168776,0.457539735933546,3.44072387544023));
#8099=CARTESIAN_POINT('Ctrl Pts',(7.2032901519641,0.527875728031689,3.4926477940433));
#8100=CARTESIAN_POINT('Ctrl Pts',(6.94079711565823,0.457422432694776,3.54439453030441));
#8101=CARTESIAN_POINT('Ctrl Pts',(6.74965929517197,0.266025262881375,3.59590534648784));
#8102=CARTESIAN_POINT('Ctrl Pts',(6.68015786626903,0.00608630836071941,
3.64713029215759));
#8103=CARTESIAN_POINT('Ctrl Pts',(6.74970359576674,-0.251928649994077,3.69801546363488));
#8104=CARTESIAN_POINT('Ctrl Pts',(6.93743508922121,-0.439308050996682,3.74852062578755));
#8105=CARTESIAN_POINT('Ctrl Pts',(7.19159056427377,-0.50709195756326,3.79860202870109));
#8106=CARTESIAN_POINT('Ctrl Pts',(7.44320748400448,-0.439333440360368,3.84822217082346));
#8107=CARTESIAN_POINT('Ctrl Pts',(7.62546589133706,-0.256624352508281,3.89734864174091));
#8108=CARTESIAN_POINT('Ctrl Pts',(7.68558445816876,-0.0305285469163073,
3.94190287089586));
#8109=CARTESIAN_POINT('Ctrl Pts',(7.64478426817293,0.172960025251268,3.98201095418908));
#8110=CARTESIAN_POINT('Ctrl Pts',(7.5418513016088,0.326832385706015,4.01779422709743));
#8111=CARTESIAN_POINT('Ctrl Pts',(7.38915121379287,0.428586196765497,4.05326072065034));
#8112=CARTESIAN_POINT('Ctrl Pts',(7.21079763277669,0.46396249107695,4.08840353362013));
#8113=CARTESIAN_POINT('Ctrl Pts',(7.03414323162941,0.428588492367169,4.12322269578801));
#8114=CARTESIAN_POINT('Ctrl Pts',(6.88581499534645,0.32933817966448,4.15771807315783));
#8115=CARTESIAN_POINT('Ctrl Pts',(6.78768181868934,0.182230564928744,4.19189009323567));
#8116=CARTESIAN_POINT('Ctrl Pts',(6.75365398677738,0.0103830219909102,4.22574466876761));
#8117=CARTESIAN_POINT('Ctrl Pts',(6.78772267677417,-0.15978639102865,4.2592862906232));
#8118=CARTESIAN_POINT('Ctrl Pts',(6.88332961654354,-0.30275014299038,4.29252038306181));
#8119=CARTESIAN_POINT('Ctrl Pts',(7.02515283508868,-0.397267137420018,4.32545966111404));
#8120=CARTESIAN_POINT('Ctrl Pts',(7.19087475875782,-0.430188336599795,4.35811115340979));
#8121=CARTESIAN_POINT('Ctrl Pts',(7.3551529846964,-0.397308309221955,4.39049217898679));
#8122=CARTESIAN_POINT('Ctrl Pts',(7.49330452445524,-0.304979351139395,4.42260903882481));
#8123=CARTESIAN_POINT('Ctrl Pts',(7.58477684160338,-0.167677553124076,4.4544919711552));
#8124=CARTESIAN_POINT('Ctrl Pts',(7.60603157928287,-0.0607527067041877,
4.47557921241636));
#8125=CARTESIAN_POINT('Ctrl Pts',(7.60603881261167,-0.00709059188521041,
4.48612173359858));
#8126=CARTESIAN_POINT('Ctrl Pts',(7.69467762570738,0.00688377669667897,
0.514991785163569));
#8127=CARTESIAN_POINT('Ctrl Pts',(7.69466889634804,0.071643808641503,0.527714615899426));
#8128=CARTESIAN_POINT('Ctrl Pts',(7.66895523814051,0.200905554952867,0.553210400550609));
#8129=CARTESIAN_POINT('Ctrl Pts',(7.55861816964784,0.36638273901977,0.591647870327449));
#8130=CARTESIAN_POINT('Ctrl Pts',(7.39259185449073,0.477265432322967,0.630241145729233));
#8131=CARTESIAN_POINT('Ctrl Pts',(7.19606255211317,0.516492063005455,0.668976010840586));
#8132=CARTESIAN_POINT('Ctrl Pts',(6.99892977540135,0.477230860818582,0.707826422052664));
#8133=CARTESIAN_POINT('Ctrl Pts',(6.83130768528331,0.365352713499376,0.746771527227674));
#8134=CARTESIAN_POINT('Ctrl Pts',(6.71925167676417,0.197519798506761,0.785785725774557));
#8135=CARTESIAN_POINT('Ctrl Pts',(6.67963411333354,-0.000791202693221011,
0.824846572270052));
#8136=CARTESIAN_POINT('Ctrl Pts',(6.71941350175141,-0.198811372269768,0.86392807407511));
#8137=CARTESIAN_POINT('Ctrl Pts',(6.86843522759788,-0.423792949454481,0.916033400754273));
#8138=CARTESIAN_POINT('Ctrl Pts',(7.19769392010731,-0.560513248480779,0.981095150002627));
#8139=CARTESIAN_POINT('Ctrl Pts',(7.52570147928999,-0.423903016810727,1.04590305884835));
#8140=CARTESIAN_POINT('Ctrl Pts',(7.67286762063526,-0.200965968483773,1.09750364116457));
#8141=CARTESIAN_POINT('Ctrl Pts',(7.72261295254984,0.0451393462758144,1.14605420709187));
#8142=CARTESIAN_POINT('Ctrl Pts',(7.61524234685028,0.340210842305179,1.20425346675242));
#8143=CARTESIAN_POINT('Ctrl Pts',(7.29912138428851,0.52136233941282,1.27174458894949));
#8144=CARTESIAN_POINT('Ctrl Pts',(6.97463054860487,0.463557001358796,1.33292698038332));
#8145=CARTESIAN_POINT('Ctrl Pts',(6.77081821446351,0.258121233797634,1.38794832985624));
#8146=CARTESIAN_POINT('Ctrl Pts',(6.70446235354691,0.0097120224784632,1.4369679279528));
#8147=CARTESIAN_POINT('Ctrl Pts',(6.77064080749259,-0.236368179035901,1.48545948666572));
#8148=CARTESIAN_POINT('Ctrl Pts',(6.94903692491188,-0.41407503667784,1.53341005809338));
#8149=CARTESIAN_POINT('Ctrl Pts',(7.18950979304665,-0.478139101185346,1.5807967612744));
#8150=CARTESIAN_POINT('Ctrl Pts',(7.4269086887867,-0.414104038473914,1.62761310972582));
#8151=CARTESIAN_POINT('Ctrl Pts',(7.59834160025041,-0.242113962547365,1.67385370366622));
#8152=CARTESIAN_POINT('Ctrl Pts',(7.66003675045965,-0.0103513232519091,
1.7195211704181));
#8153=CARTESIAN_POINT('Ctrl Pts',(7.59836117318194,0.218336823777539,1.76462300661926));
#8154=CARTESIAN_POINT('Ctrl Pts',(7.43265726637053,0.383504832459041,1.80917303346396));
#8155=CARTESIAN_POINT('Ctrl Pts',(7.20928361949127,0.442992153199741,1.85319029170689));
#8156=CARTESIAN_POINT('Ctrl Pts',(6.98863987248015,0.38351198596622,1.89669991461219));
#8157=CARTESIAN_POINT('Ctrl Pts',(6.82910226668574,0.223518600666567,1.93973098682015));
#8158=CARTESIAN_POINT('Ctrl Pts',(6.77139704108765,0.00734290766390798,
1.98232025113029));
#8159=CARTESIAN_POINT('Ctrl Pts',(6.81955140322323,-0.17080763583515,2.01747249154634));
#8160=CARTESIAN_POINT('Ctrl Pts',(6.90677940492032,-0.284130764144419,2.0454129068512));
#8161=CARTESIAN_POINT('Ctrl Pts',(7.01970141686137,-0.370956746763405,2.07324122060183));
#8162=CARTESIAN_POINT('Ctrl Pts',(7.19517285585778,-0.417865627882994,2.10783440889197));
#8163=CARTESIAN_POINT('Ctrl Pts',(7.40439082299913,-0.361726044210867,2.14907886919864));
#8164=CARTESIAN_POINT('Ctrl Pts',(7.55671510006043,-0.209184076105135,2.19011719492698));
#8165=CARTESIAN_POINT('Ctrl Pts',(7.60748456033901,-0.0190531027858145,
2.22759299177402));
#8166=CARTESIAN_POINT('Ctrl Pts',(7.57300852841629,0.153433881101946,2.26158938023144));
#8167=CARTESIAN_POINT('Ctrl Pts',(7.48522152825439,0.284973433685168,2.29215525097081));
#8168=CARTESIAN_POINT('Ctrl Pts',(7.35371479002735,0.37272858905955,2.32271540904616));
#8169=CARTESIAN_POINT('Ctrl Pts',(7.18132429762203,0.407224317027577,2.35669104556836));
#8170=CARTESIAN_POINT('Ctrl Pts',(6.9913809597726,0.356397258300469,2.39412528364257));
#8171=CARTESIAN_POINT('Ctrl Pts',(6.83922114282842,0.204287390367652,2.43509680013667));
#8172=CARTESIAN_POINT('Ctrl Pts',(6.78776554029098,0.0128275311884052,2.47282559318833));
#8173=CARTESIAN_POINT('Ctrl Pts',(6.82279513668012,-0.161901812992041,2.50730303808298));
#8174=CARTESIAN_POINT('Ctrl Pts',(6.94158088523551,-0.34159342973453,2.54888699780782));
#8175=CARTESIAN_POINT('Ctrl Pts',(7.20629039228909,-0.452427791333231,2.60131567268228));
#8176=CARTESIAN_POINT('Ctrl Pts',(7.5304300988666,-0.319328872462905,2.66510484392403));
#8177=CARTESIAN_POINT('Ctrl Pts',(7.64393545484647,-0.0463609609462171,
2.71910010788248));
#8178=CARTESIAN_POINT('Ctrl Pts',(7.59909834565696,0.175907590184711,2.76286026063545));
#8179=CARTESIAN_POINT('Ctrl Pts',(7.50438991288635,0.318409515321193,2.79597016810716));
#8180=CARTESIAN_POINT('Ctrl Pts',(7.3605799039455,0.414556437496516,2.82938176955588));
#8181=CARTESIAN_POINT('Ctrl Pts',(7.18955265969801,0.448811059922502,2.86310195270141));
#8182=CARTESIAN_POINT('Ctrl Pts',(7.01678655931437,0.414550262799124,2.89713771190015));
#8183=CARTESIAN_POINT('Ctrl Pts',(6.86885174085118,0.315990474399967,2.93149384807802));
#8184=CARTESIAN_POINT('Ctrl Pts',(6.76911069802026,0.166845046570867,2.96617128633524));
#8185=CARTESIAN_POINT('Ctrl Pts',(6.72953139858562,-0.0304522148375183,
3.00506495776769));
#8186=CARTESIAN_POINT('Ctrl Pts',(6.78769390474188,-0.249937774164215,3.04830039529776));
#8187=CARTESIAN_POINT('Ctrl Pts',(6.9649370626522,-0.427422514214055,3.09603683868771));
#8188=CARTESIAN_POINT('Ctrl Pts',(7.18932018203905,-0.487979620328074,3.14030064536012));
#8189=CARTESIAN_POINT('Ctrl Pts',(7.39557279768717,-0.446904315163521,3.18093085548355));
#8190=CARTESIAN_POINT('Ctrl Pts',(7.55425360364287,-0.341191109504664,3.21778878121054));
#8191=CARTESIAN_POINT('Ctrl Pts',(7.66102690207568,-0.181435475111084,3.25492379188564));
#8192=CARTESIAN_POINT('Ctrl Pts',(7.70328741298565,0.0294016985791167,3.2964816011759));
#8193=CARTESIAN_POINT('Ctrl Pts',(7.64104047721324,0.263177246401401,3.34254524203817));
#8194=CARTESIAN_POINT('Ctrl Pts',(7.45302343605178,0.451617524859523,3.39320364580977));
#8195=CARTESIAN_POINT('Ctrl Pts',(7.19421186989991,0.521059884552374,3.44422754118507));
#8196=CARTESIAN_POINT('Ctrl Pts',(6.93366759288141,0.451480374799088,3.49556420787452));
#8197=CARTESIAN_POINT('Ctrl Pts',(6.74192572911501,0.259952952462136,3.54716607559634));
#8198=CARTESIAN_POINT('Ctrl Pts',(6.67128705932614,-0.00291987582538055,
3.59897914569118));
#8199=CARTESIAN_POINT('Ctrl Pts',(6.74200130890162,-0.266556153752997,3.65095085469123));
#8200=CARTESIAN_POINT('Ctrl Pts',(6.93533270564664,-0.459989954442243,3.70302170351135));
#8201=CARTESIAN_POINT('Ctrl Pts',(7.19973042361935,-0.530836528881026,3.75513473434544));
#8202=CARTESIAN_POINT('Ctrl Pts',(7.46399256228725,-0.459988881699339,3.80723200840435));
#8203=CARTESIAN_POINT('Ctrl Pts',(7.65720752588036,-0.266714233190792,3.85925510262137));
#8204=CARTESIAN_POINT('Ctrl Pts',(7.72162850029991,-0.0253919365293239,
3.90682319346266));
#8205=CARTESIAN_POINT('Ctrl Pts',(7.67789482230646,0.193331762568851,3.94992933060867));
#8206=CARTESIAN_POINT('Ctrl Pts',(7.56675267456708,0.359645580693078,3.98859787225562));
#8207=CARTESIAN_POINT('Ctrl Pts',(7.40097626920353,0.47022490567555,4.02711395823539));
#8208=CARTESIAN_POINT('Ctrl Pts',(7.20640719990281,0.508899267550811,4.06545972626007));
#8209=CARTESIAN_POINT('Ctrl Pts',(7.01283946983003,0.470213246623792,4.1036131517629));
#8210=CARTESIAN_POINT('Ctrl Pts',(6.84967688295545,0.36111126628715,4.1415548777527));
#8211=CARTESIAN_POINT('Ctrl Pts',(6.74134731945609,0.198812605531192,4.17926855876961));
#8212=CARTESIAN_POINT('Ctrl Pts',(6.70365533298111,0.00866379922224738,
4.21673517440635));
#8213=CARTESIAN_POINT('Ctrl Pts',(6.74140931659415,-0.180078545667991,4.25394103083648));
#8214=CARTESIAN_POINT('Ctrl Pts',(6.84762388733812,-0.338921159861923,4.29087272651501));
#8215=CARTESIAN_POINT('Ctrl Pts',(7.00537067407869,-0.444065320510892,4.3275172120746));
#8216=CARTESIAN_POINT('Ctrl Pts',(7.18981724442161,-0.480695590575098,4.36386348999543));
#8217=CARTESIAN_POINT('Ctrl Pts',(7.37263926416229,-0.444099896756117,4.399905298103));
#8218=CARTESIAN_POINT('Ctrl Pts',(7.52627543630935,-0.341400177175117,4.43562905755834));
#8219=CARTESIAN_POINT('Ctrl Pts',(7.62785720298341,-0.188901379750348,4.47104576944789));
#8220=CARTESIAN_POINT('Ctrl Pts',(7.65140397112763,-0.0703858575854634,
4.49442272113103));
#8221=CARTESIAN_POINT('Ctrl Pts',(7.6514119734328,-0.0110189146175235,4.50608601945378));
#8222=CARTESIAN_POINT('Ctrl Pts',(7.66495866561397,0.0096408208356154,0.500937861339137));
#8223=CARTESIAN_POINT('Ctrl Pts',(7.66495043542855,0.0706976578322391,0.512933158114727));
#8224=CARTESIAN_POINT('Ctrl Pts',(7.6407288414539,0.192578461749219,0.53697092906723));
#8225=CARTESIAN_POINT('Ctrl Pts',(7.53641483655384,0.349135128226674,0.57332721437664));
#8226=CARTESIAN_POINT('Ctrl Pts',(7.37891862529407,0.454388959539344,0.609942269987145));
#8227=CARTESIAN_POINT('Ctrl Pts',(7.19182916610252,0.491804928705749,0.646817568764298));
#8228=CARTESIAN_POINT('Ctrl Pts',(7.00345300936995,0.454364611540757,0.683937116394234));
#8229=CARTESIAN_POINT('Ctrl Pts',(6.8426331207003,0.347126595132945,0.72128862247113));
#8230=CARTESIAN_POINT('Ctrl Pts',(6.73465279105392,0.185548007545082,0.758857805369577));
#8231=CARTESIAN_POINT('Ctrl Pts',(6.69624812122046,-0.00620356043593041,
0.796628033574345));
#8232=CARTESIAN_POINT('Ctrl Pts',(6.73480718344848,-0.198554484110674,0.834582940724046));
#8233=CARTESIAN_POINT('Ctrl Pts',(6.88005293713107,-0.418084886861934,0.885411952478362));
#8234=CARTESIAN_POINT('Ctrl Pts',(7.20322101675746,-0.552973672355533,0.949310201794791));
#8235=CARTESIAN_POINT('Ctrl Pts',(7.52875135792009,-0.418120197994963,1.01356942995885));
#8236=CARTESIAN_POINT('Ctrl Pts',(7.67590748900772,-0.195467714230404,1.06510280128326));
#8237=CARTESIAN_POINT('Ctrl Pts',(7.72594697491113,0.051510497628374,1.11382936475781));
#8238=CARTESIAN_POINT('Ctrl Pts',(7.61792973454696,0.34980833854487,1.17261054327264));
#8239=CARTESIAN_POINT('Ctrl Pts',(7.29600845579134,0.534934534966306,1.24137836329612));
#8240=CARTESIAN_POINT('Ctrl Pts',(6.9624343826518,0.475986238152519,1.30425389372148));
#8241=CARTESIAN_POINT('Ctrl Pts',(6.7513269732076,0.263559075549507,1.36117052033831));
#8242=CARTESIAN_POINT('Ctrl Pts',(6.68208673935486,0.00506624913794415,
1.41217539507843));
#8243=CARTESIAN_POINT('Ctrl Pts',(6.75115729338842,-0.252515030784761,1.46291637360071));
#8244=CARTESIAN_POINT('Ctrl Pts',(6.93868139789632,-0.439549141627597,1.51333206514984));
#8245=CARTESIAN_POINT('Ctrl Pts',(7.19277218532913,-0.507400915671182,1.56339686963768));
#8246=CARTESIAN_POINT('Ctrl Pts',(7.44475704014889,-0.439568775677871,1.6130666625822));
#8247=CARTESIAN_POINT('Ctrl Pts',(7.62746056234528,-0.256432683273915,1.66231123683637));
#8248=CARTESIAN_POINT('Ctrl Pts',(7.69348210450095,-0.00877779198086032,
1.71110033955553));
#8249=CARTESIAN_POINT('Ctrl Pts',(7.62746910095865,0.236264427972525,1.75941038595882));
#8250=CARTESIAN_POINT('Ctrl Pts',(7.44962012238075,0.413605394268341,1.80722176291839));
#8251=CARTESIAN_POINT('Ctrl Pts',(7.20954044812925,0.477565743583523,1.85452048529808));
#8252=CARTESIAN_POINT('Ctrl Pts',(6.97227231959396,0.413602123353752,1.90129735375243));
#8253=CARTESIAN_POINT('Ctrl Pts',(6.80077909361189,0.241579533289261,1.94754921821389));
#8254=CARTESIAN_POINT('Ctrl Pts',(6.7388618673047,0.00940863316150851,1.9932768407136));
#8255=CARTESIAN_POINT('Ctrl Pts',(6.79054491525727,-0.181541982999997,2.03095403885583));
#8256=CARTESIAN_POINT('Ctrl Pts',(6.88387815366437,-0.302767035565214,2.06084460346816));
#8257=CARTESIAN_POINT('Ctrl Pts',(7.00451694241951,-0.395503980057399,2.09056986286438));
#8258=CARTESIAN_POINT('Ctrl Pts',(7.19149482154426,-0.445378090698615,2.1274222004115));
#8259=CARTESIAN_POINT('Ctrl Pts',(7.41343391189553,-0.385678179322762,2.17118156013989));
#8260=CARTESIAN_POINT('Ctrl Pts',(7.57412088328951,-0.224511384987361,2.21450495485577));
#8261=CARTESIAN_POINT('Ctrl Pts',(7.62724779211325,-0.0248721738545197,
2.25384933801546));
#8262=CARTESIAN_POINT('Ctrl Pts',(7.59116361468395,0.155190246720775,2.28934298364047));
#8263=CARTESIAN_POINT('Ctrl Pts',(7.49989052392447,0.291790939188551,2.32109884315156));
#8264=CARTESIAN_POINT('Ctrl Pts',(7.36395007742405,0.38239718016914,2.35268032633859));
#8265=CARTESIAN_POINT('Ctrl Pts',(7.18676166604564,0.417742312375305,2.38759960338815));
#8266=CARTESIAN_POINT('Ctrl Pts',(6.99291266772421,0.365648667519335,2.42582318365208));
#8267=CARTESIAN_POINT('Ctrl Pts',(6.83897107184478,0.211431047408248,2.46732314866766));
#8268=CARTESIAN_POINT('Ctrl Pts',(6.78748883973987,0.0190035426787835,2.50524603217002));
#8269=CARTESIAN_POINT('Ctrl Pts',(6.82252928042011,-0.155278930965659,2.53965006117662));
#8270=CARTESIAN_POINT('Ctrl Pts',(6.94047269326526,-0.333425126549853,2.58089918196454));
#8271=CARTESIAN_POINT('Ctrl Pts',(7.20090707643882,-0.441779652078452,2.63244776860263));
#8272=CARTESIAN_POINT('Ctrl Pts',(7.51563071205169,-0.311721566968956,2.69446142088775));
#8273=CARTESIAN_POINT('Ctrl Pts',(7.62430311252255,-0.0489647930063533,
2.74642328448686));
#8274=CARTESIAN_POINT('Ctrl Pts',(7.5813840421979,0.163308287319331,2.78823405894546));
#8275=CARTESIAN_POINT('Ctrl Pts',(7.49123285044309,0.298833086231118,2.81973896360247));
#8276=CARTESIAN_POINT('Ctrl Pts',(7.35493116122275,0.389891719124265,2.85140756747005));
#8277=CARTESIAN_POINT('Ctrl Pts',(7.19341536220524,0.422180171213018,2.88325853512063));
#8278=CARTESIAN_POINT('Ctrl Pts',(7.03077842930683,0.389887859695428,2.91530957463356));
#8279=CARTESIAN_POINT('Ctrl Pts',(6.89190449463321,0.297309810814242,2.94757450110591));
#8280=CARTESIAN_POINT('Ctrl Pts',(6.79848642055615,0.157571536298674,2.98007238787189));
#8281=CARTESIAN_POINT('Ctrl Pts',(6.76150685487504,-0.0269250762532582,
3.01644525951301));
#8282=CARTESIAN_POINT('Ctrl Pts',(6.81585071674324,-0.231845001847761,3.05683113794882));
#8283=CARTESIAN_POINT('Ctrl Pts',(6.98114939225645,-0.397360174681789,3.101361111042));
#8284=CARTESIAN_POINT('Ctrl Pts',(7.19033341376853,-0.453815928881707,3.14263718537585));
#8285=CARTESIAN_POINT('Ctrl Pts',(7.38267033377326,-0.415535666902471,3.18053365000396));
#8286=CARTESIAN_POINT('Ctrl Pts',(7.5307464143918,-0.316904538681263,3.21493081649486));
#8287=CARTESIAN_POINT('Ctrl Pts',(7.63050738643256,-0.167696568139501,3.24962471887291));
#8288=CARTESIAN_POINT('Ctrl Pts',(7.67006526296691,0.0295052786481756,3.28849853708803));
#8289=CARTESIAN_POINT('Ctrl Pts',(7.61180808226649,0.248648829409802,3.3316858887866));
#8290=CARTESIAN_POINT('Ctrl Pts',(7.43514984947071,0.425869407836813,3.37931317995539));
#8291=CARTESIAN_POINT('Ctrl Pts',(7.19106330905834,0.491496622933082,3.42744471708512));
#8292=CARTESIAN_POINT('Ctrl Pts',(6.94429664016134,0.425752312282669,3.47606216769791));
#8293=CARTESIAN_POINT('Ctrl Pts',(6.76180911767831,0.243701545752318,3.52514523794754));
#8294=CARTESIAN_POINT('Ctrl Pts',(6.69412136518916,-0.00747982371833415,
3.57466354176041));
#8295=CARTESIAN_POINT('Ctrl Pts',(6.76187382592234,-0.260799521439724,3.62459127426534));
#8296=CARTESIAN_POINT('Ctrl Pts',(6.94847611579586,-0.447791932889458,3.67488482395855));
#8297=CARTESIAN_POINT('Ctrl Pts',(7.20529145918771,-0.516830252602251,3.72550931504893));
#8298=CARTESIAN_POINT('Ctrl Pts',(7.46363123050322,-0.447802422833225,3.77642000140872));
#8299=CARTESIAN_POINT('Ctrl Pts',(7.6538074437744,-0.257897177129994,3.82757293127415));
#8300=CARTESIAN_POINT('Ctrl Pts',(7.7177715912926,-0.0191264507767671,3.8746366938418));
#8301=CARTESIAN_POINT('Ctrl Pts',(7.67435473390573,0.198582385366778,3.91753173887265));
#8302=CARTESIAN_POINT('Ctrl Pts',(7.56329681060452,0.364957935365554,3.95619050975397));
#8303=CARTESIAN_POINT('Ctrl Pts',(7.39675108803321,0.476165093095772,3.99489365541533));
#8304=CARTESIAN_POINT('Ctrl Pts',(7.20029814145452,0.515321267550363,4.03360638733665));
#8305=CARTESIAN_POINT('Ctrl Pts',(7.00387047286649,0.476163919411364,4.07231102869526));
#8306=CARTESIAN_POINT('Ctrl Pts',(6.83746567537909,0.365016133595194,4.11098698220102));
#8307=CARTESIAN_POINT('Ctrl Pts',(6.72642378886519,0.198833317396287,4.14960586405847));
#8308=CARTESIAN_POINT('Ctrl Pts',(6.68753839413938,0.00317933679133277,
4.18815341806877));
#8309=CARTESIAN_POINT('Ctrl Pts',(6.72647710351975,-0.191933239252609,4.22660331585192));
#8310=CARTESIAN_POINT('Ctrl Pts',(6.83665572362076,-0.356887001441586,4.2649335303692));
#8311=CARTESIAN_POINT('Ctrl Pts',(7.00106911490509,-0.466565590640207,4.30312749646998));
#8312=CARTESIAN_POINT('Ctrl Pts',(7.19410690234209,-0.504987935840618,4.34116313228386));
#8313=CARTESIAN_POINT('Ctrl Pts',(7.38621803807239,-0.466593360436696,4.37902453826879));
#8314=CARTESIAN_POINT('Ctrl Pts',(7.54825768185721,-0.3583357834793,4.4166899096587));
#8315=CARTESIAN_POINT('Ctrl Pts',(7.65577203010817,-0.197002467064972,4.4541521298834));
#8316=CARTESIAN_POINT('Ctrl Pts',(7.6807779728439,-0.0711713717257019,4.47896571871842));
#8317=CARTESIAN_POINT('Ctrl Pts',(7.68078647070003,-0.00812806991155192,
4.49135127875486));
#8318=CARTESIAN_POINT('Ctrl Pts',(7.64999870073278,0.00963880430002493,
0.500937861339137));
#8319=CARTESIAN_POINT('Ctrl Pts',(7.64999072283273,0.0688240253405825,0.512565458280486));
#8320=CARTESIAN_POINT('Ctrl Pts',(7.62651906829351,0.186933280416436,0.535860737255745));
#8321=CARTESIAN_POINT('Ctrl Pts',(7.52538952050926,0.338721501716328,0.571111621876026));
#8322=CARTESIAN_POINT('Ctrl Pts',(7.37261016576107,0.440828782725881,0.606632113855559));
#8323=CARTESIAN_POINT('Ctrl Pts',(7.19098801918939,0.477160089388571,0.642432691908446));
#8324=CARTESIAN_POINT('Ctrl Pts',(7.00794887133667,0.440792445335284,0.678501299793522));
#8325=CARTESIAN_POINT('Ctrl Pts',(6.85151949944076,0.336499171833787,0.714833893830788));
#8326=CARTESIAN_POINT('Ctrl Pts',(6.74635289761356,0.179164878106423,0.751420068859459));
#8327=CARTESIAN_POINT('Ctrl Pts',(6.7088855037237,-0.00779582609077112,
0.78825059826266));
#8328=CARTESIAN_POINT('Ctrl Pts',(6.74651391108833,-0.195622387289353,0.825313313466632));
#8329=CARTESIAN_POINT('Ctrl Pts',(6.88851119015049,-0.410310488976418,0.875022999496246));
#8330=CARTESIAN_POINT('Ctrl Pts',(7.20522985356176,-0.542753193552164,0.937673401670968));
#8331=CARTESIAN_POINT('Ctrl Pts',(7.52560124560565,-0.410308950963103,1.00090311405878));
#8332=CARTESIAN_POINT('Ctrl Pts',(7.67086762315913,-0.190619832396083,1.0517623380234));
#8333=CARTESIAN_POINT('Ctrl Pts',(7.72038428103372,0.053554354178951,1.09994516441643));
#8334=CARTESIAN_POINT('Ctrl Pts',(7.61346157902179,0.349425527858921,1.15825605943124));
#8335=CARTESIAN_POINT('Ctrl Pts',(7.293147036645,0.533923363778534,1.22671892603372));
#8336=CARTESIAN_POINT('Ctrl Pts',(6.9598052915743,0.475238618295502,1.28954716027338));
#8337=CARTESIAN_POINT('Ctrl Pts',(6.74803078150055,0.262318163018047,1.34663189357301));
#8338=CARTESIAN_POINT('Ctrl Pts',(6.67830810206772,0.0023988076890563,1.3979329504908));
#8339=CARTESIAN_POINT('Ctrl Pts',(6.74786353789082,-0.257385664114871,1.44910892564238));
#8340=CARTESIAN_POINT('Ctrl Pts',(6.93745136291826,-0.446625861944449,1.50011118169226));
#8341=CARTESIAN_POINT('Ctrl Pts',(7.19511270617401,-0.515530236866011,1.55089291586215));
#8342=CARTESIAN_POINT('Ctrl Pts',(7.45136837615866,-0.446648689171563,1.60140954707133));
#8343=CARTESIAN_POINT('Ctrl Pts',(7.63768442718454,-0.260018056286165,1.65161922462518));
#8344=CARTESIAN_POINT('Ctrl Pts',(7.70523033687804,-0.0069714683683192,
1.70148323387221));
#8345=CARTESIAN_POINT('Ctrl Pts',(7.63769895751989,0.244003419049979,1.75096640161628));
#8346=CARTESIAN_POINT('Ctrl Pts',(7.45523859330254,0.426040600914326,1.80003745460796));
#8347=CARTESIAN_POINT('Ctrl Pts',(7.20843773134158,0.491855409637758,1.84866933496872));
#8348=CARTESIAN_POINT('Ctrl Pts',(6.96411419073211,0.426044527968114,1.89683949153479));
#8349=CARTESIAN_POINT('Ctrl Pts',(6.7872702247347,0.248717255937941,1.94453007704133));
#8350=CARTESIAN_POINT('Ctrl Pts',(6.72333142706999,0.00910740273079913,
1.99172820696913));
#8351=CARTESIAN_POINT('Ctrl Pts',(6.77669190792476,-0.188112629887261,2.03064296753181));
#8352=CARTESIAN_POINT('Ctrl Pts',(6.87311288530633,-0.313353108724919,2.06152326719269));
#8353=CARTESIAN_POINT('Ctrl Pts',(6.9977575234091,-0.409174440391491,2.0922362142172));
#8354=CARTESIAN_POINT('Ctrl Pts',(7.19095586866206,-0.460713817161615,2.13031448846159));
#8355=CARTESIAN_POINT('Ctrl Pts',(7.42021304552618,-0.399036009194613,2.17551521533059));
#8356=CARTESIAN_POINT('Ctrl Pts',(7.58607675038944,-0.232652998639623,2.22023530187249));
#8357=CARTESIAN_POINT('Ctrl Pts',(7.64084113722653,-0.0267711157317457,
2.2608041635776));
#8358=CARTESIAN_POINT('Ctrl Pts',(7.60365245023964,0.158696418911201,2.2973634945418));
#8359=CARTESIAN_POINT('Ctrl Pts',(7.50973838584388,0.299219822341778,2.33003006433835));
#8360=CARTESIAN_POINT('Ctrl Pts',(7.37007100234203,0.392281683236922,2.36247215334549));
#8361=CARTESIAN_POINT('Ctrl Pts',(7.18832364110351,0.428509871500047,2.39828479951764));
#8362=CARTESIAN_POINT('Ctrl Pts',(6.98993152312495,0.375130255900093,2.43739940337039));
#8363=CARTESIAN_POINT('Ctrl Pts',(6.83283942785452,0.217642962930976,2.47976008769737));
#8364=CARTESIAN_POINT('Ctrl Pts',(6.7805179762894,0.0217759129571612,2.51834494637949));
#8365=CARTESIAN_POINT('Ctrl Pts',(6.81611962546049,-0.155110783437508,2.55325894844757));
#8366=CARTESIAN_POINT('Ctrl Pts',(6.93559514558806,-0.335467183812974,2.59501419582854));
#8367=CARTESIAN_POINT('Ctrl Pts',(7.19838636703693,-0.444497554803198,2.64699296075227));
#8368=CARTESIAN_POINT('Ctrl Pts',(7.51396784981042,-0.313675439428632,2.70919005501935));
#8369=CARTESIAN_POINT('Ctrl Pts',(7.62212313812957,-0.0514208051434247,
2.76101600110827));
#8370=CARTESIAN_POINT('Ctrl Pts',(7.57941022831611,0.159498854704775,2.80255943176652));
#8371=CARTESIAN_POINT('Ctrl Pts',(7.49002790476542,0.293811387305209,2.83377939972915));
#8372=CARTESIAN_POINT('Ctrl Pts',(7.3552499441484,0.383795703607156,2.86508254302445));
#8373=CARTESIAN_POINT('Ctrl Pts',(7.19595280633545,0.41560735445773,2.89648910888395));
#8374=CARTESIAN_POINT('Ctrl Pts',(7.03593949389396,0.383792650446306,2.92801879141503));
#8375=CARTESIAN_POINT('Ctrl Pts',(6.89961651509014,0.292876470296345,2.95969053299985));
#8376=CARTESIAN_POINT('Ctrl Pts',(6.8081238548802,0.155952445855146,2.99152250722056));
#8377=CARTESIAN_POINT('Ctrl Pts',(6.7719951154116,-0.0244720795860329,3.02708849903104));
#8378=CARTESIAN_POINT('Ctrl Pts',(6.82508694038131,-0.224423780156864,3.0664872528009));
#8379=CARTESIAN_POINT('Ctrl Pts',(6.9861130399098,-0.385566648672682,3.1098474493302));
#8380=CARTESIAN_POINT('Ctrl Pts',(7.18949761386412,-0.440411898981026,3.14997109794484));
#8381=CARTESIAN_POINT('Ctrl Pts',(7.37626527013998,-0.403213775048244,3.18676673081186));
#8382=CARTESIAN_POINT('Ctrl Pts',(7.51993103796524,-0.30750405465344,3.2201390303787));
#8383=CARTESIAN_POINT('Ctrl Pts',(7.61665044076158,-0.16281791922389,3.25377599756719));
#8384=CARTESIAN_POINT('Ctrl Pts',(7.65498225700094,0.0283123086785322,3.29145196922942));
#8385=CARTESIAN_POINT('Ctrl Pts',(7.59852316170633,0.240631420079613,3.3332902111484));
#8386=CARTESIAN_POINT('Ctrl Pts',(7.42736589163809,0.412328652603764,3.37943210760514));
#8387=CARTESIAN_POINT('Ctrl Pts',(7.19081184831391,0.475941162716025,3.42607713455886));
#8388=CARTESIAN_POINT('Ctrl Pts',(6.95151342469985,0.412204069493947,3.47322302929114));
#8389=CARTESIAN_POINT('Ctrl Pts',(6.77437422620912,0.235528496642651,3.52086247665056));
#8390=CARTESIAN_POINT('Ctrl Pts',(6.70856719057301,-0.00853695568196444,
3.56898306053165));
#8391=CARTESIAN_POINT('Ctrl Pts',(6.77444746404088,-0.255049338492359,3.61756749823055));
#8392=CARTESIAN_POINT('Ctrl Pts',(6.9562898685306,-0.437346140614658,3.66659366870206));
#8393=CARTESIAN_POINT('Ctrl Pts',(7.20705837195632,-0.504822359013845,3.71603499825878));
#8394=CARTESIAN_POINT('Ctrl Pts',(7.45987118758895,-0.437340247483335,3.76586064283255));
#8395=CARTESIAN_POINT('Ctrl Pts',(7.64643847266503,-0.251145802482984,3.81603581337119));
#8396=CARTESIAN_POINT('Ctrl Pts',(7.70939130979041,-0.0164226811455054,
3.86231497498143));
#8397=CARTESIAN_POINT('Ctrl Pts',(7.66665300702434,0.198091300428752,3.90458351454994));
#8398=CARTESIAN_POINT('Ctrl Pts',(7.55703831361006,0.362363180751678,3.94275824199772));
#8399=CARTESIAN_POINT('Ctrl Pts',(7.39231161872226,0.472405147713809,3.98104671473859));
#8400=CARTESIAN_POINT('Ctrl Pts',(7.19757748614764,0.511253819560404,4.01942894411337));
#8401=CARTESIAN_POINT('Ctrl Pts',(7.00243742159468,0.472394913482402,4.05788442705078));
#8402=CARTESIAN_POINT('Ctrl Pts',(6.83675859423202,0.361776141956741,4.09639221672569));
#8403=CARTESIAN_POINT('Ctrl Pts',(6.72593678453896,0.195994806221917,4.13493108529455));
#8404=CARTESIAN_POINT('Ctrl Pts',(6.6870196897812,0.000372767277272366,
4.17347960299015));
#8405=CARTESIAN_POINT('Ctrl Pts',(6.72599808190112,-0.19515902350661,4.21201632288769));
#8406=CARTESIAN_POINT('Ctrl Pts',(6.83662574734572,-0.360840864201945,4.25051978478148));
#8407=CARTESIAN_POINT('Ctrl Pts',(7.00208504736442,-0.47127212461887,4.28896891774833));
#8408=CARTESIAN_POINT('Ctrl Pts',(7.19679737636779,-0.510060779189973,4.32734248506513));
#8409=CARTESIAN_POINT('Ctrl Pts',(7.39100313831524,-0.471299286801184,4.36562087591661));
#8410=CARTESIAN_POINT('Ctrl Pts',(7.5551719819179,-0.361667391724164,4.40378216412631));
#8411=CARTESIAN_POINT('Ctrl Pts',(7.66435033350436,-0.197951056928272,4.44181269280615));
#8412=CARTESIAN_POINT('Ctrl Pts',(7.68982126235038,-0.0699660743691742,
4.46705762798012));
#8413=CARTESIAN_POINT('Ctrl Pts',(7.68982990724746,-0.00583191542195246,
4.4796574990714));
#8414=CARTESIAN_POINT('',(7.64999870073278,0.00963880430002493,0.500937861339137));
#8415=CARTESIAN_POINT('Origin',(7.65,-1.95245324213388E-18,0.55));
#8416=CARTESIAN_POINT('',(7.68982990724746,-0.00583191542195245,4.4796574990714));
#8417=CARTESIAN_POINT('Ctrl Pts',(7.64999870073278,0.00963880430002493,
0.500937861339137));
#8418=CARTESIAN_POINT('Ctrl Pts',(7.64999072283273,0.0688240253405825,0.512565458280486));
#8419=CARTESIAN_POINT('Ctrl Pts',(7.62651906829351,0.186933280416436,0.535860737255745));
#8420=CARTESIAN_POINT('Ctrl Pts',(7.52538952050926,0.338721501716328,0.571111621876026));
#8421=CARTESIAN_POINT('Ctrl Pts',(7.37261016576107,0.440828782725881,0.606632113855559));
#8422=CARTESIAN_POINT('Ctrl Pts',(7.19098801918939,0.477160089388571,0.642432691908446));
#8423=CARTESIAN_POINT('Ctrl Pts',(7.00794887133667,0.440792445335284,0.678501299793522));
#8424=CARTESIAN_POINT('Ctrl Pts',(6.85151949944076,0.336499171833787,0.714833893830788));
#8425=CARTESIAN_POINT('Ctrl Pts',(6.74635289761356,0.179164878106423,0.751420068859459));
#8426=CARTESIAN_POINT('Ctrl Pts',(6.7088855037237,-0.00779582609077112,
0.78825059826266));
#8427=CARTESIAN_POINT('Ctrl Pts',(6.74651391108833,-0.195622387289353,0.825313313466632));
#8428=CARTESIAN_POINT('Ctrl Pts',(6.88851119015049,-0.410310488976418,0.875022999496246));
#8429=CARTESIAN_POINT('Ctrl Pts',(7.20522985356176,-0.542753193552164,0.937673401670968));
#8430=CARTESIAN_POINT('Ctrl Pts',(7.52560124560565,-0.410308950963103,1.00090311405878));
#8431=CARTESIAN_POINT('Ctrl Pts',(7.67086762315913,-0.190619832396083,1.0517623380234));
#8432=CARTESIAN_POINT('Ctrl Pts',(7.72038428103372,0.053554354178951,1.09994516441643));
#8433=CARTESIAN_POINT('Ctrl Pts',(7.61346157902179,0.349425527858921,1.15825605943124));
#8434=CARTESIAN_POINT('Ctrl Pts',(7.293147036645,0.533923363778534,1.22671892603372));
#8435=CARTESIAN_POINT('Ctrl Pts',(6.9598052915743,0.475238618295502,1.28954716027338));
#8436=CARTESIAN_POINT('Ctrl Pts',(6.74803078150055,0.262318163018047,1.34663189357301));
#8437=CARTESIAN_POINT('Ctrl Pts',(6.67830810206772,0.0023988076890563,1.3979329504908));
#8438=CARTESIAN_POINT('Ctrl Pts',(6.74786353789082,-0.257385664114871,1.44910892564238));
#8439=CARTESIAN_POINT('Ctrl Pts',(6.93745136291826,-0.446625861944449,1.50011118169226));
#8440=CARTESIAN_POINT('Ctrl Pts',(7.19511270617401,-0.515530236866011,1.55089291586215));
#8441=CARTESIAN_POINT('Ctrl Pts',(7.45136837615866,-0.446648689171563,1.60140954707133));
#8442=CARTESIAN_POINT('Ctrl Pts',(7.63768442718454,-0.260018056286165,1.65161922462518));
#8443=CARTESIAN_POINT('Ctrl Pts',(7.70523033687804,-0.0069714683683192,
1.70148323387221));
#8444=CARTESIAN_POINT('Ctrl Pts',(7.63769895751989,0.244003419049979,1.75096640161628));
#8445=CARTESIAN_POINT('Ctrl Pts',(7.45523859330254,0.426040600914326,1.80003745460796));
#8446=CARTESIAN_POINT('Ctrl Pts',(7.20843773134158,0.491855409637758,1.84866933496872));
#8447=CARTESIAN_POINT('Ctrl Pts',(6.96411419073211,0.426044527968114,1.89683949153479));
#8448=CARTESIAN_POINT('Ctrl Pts',(6.7872702247347,0.248717255937941,1.94453007704133));
#8449=CARTESIAN_POINT('Ctrl Pts',(6.72333142706999,0.00910740273079913,
1.99172820696913));
#8450=CARTESIAN_POINT('Ctrl Pts',(6.77669190792476,-0.188112629887261,2.03064296753181));
#8451=CARTESIAN_POINT('Ctrl Pts',(6.87311288530633,-0.313353108724919,2.06152326719269));
#8452=CARTESIAN_POINT('Ctrl Pts',(6.9977575234091,-0.409174440391491,2.0922362142172));
#8453=CARTESIAN_POINT('Ctrl Pts',(7.19095586866206,-0.460713817161615,2.13031448846159));
#8454=CARTESIAN_POINT('Ctrl Pts',(7.42021304552618,-0.399036009194613,2.17551521533059));
#8455=CARTESIAN_POINT('Ctrl Pts',(7.58607675038944,-0.232652998639623,2.22023530187249));
#8456=CARTESIAN_POINT('Ctrl Pts',(7.64084113722653,-0.0267711157317457,
2.2608041635776));
#8457=CARTESIAN_POINT('Ctrl Pts',(7.60365245023964,0.158696418911201,2.2973634945418));
#8458=CARTESIAN_POINT('Ctrl Pts',(7.50973838584388,0.299219822341778,2.33003006433835));
#8459=CARTESIAN_POINT('Ctrl Pts',(7.37007100234203,0.392281683236922,2.36247215334549));
#8460=CARTESIAN_POINT('Ctrl Pts',(7.18832364110351,0.428509871500047,2.39828479951764));
#8461=CARTESIAN_POINT('Ctrl Pts',(6.98993152312495,0.375130255900093,2.43739940337039));
#8462=CARTESIAN_POINT('Ctrl Pts',(6.83283942785452,0.217642962930976,2.47976008769737));
#8463=CARTESIAN_POINT('Ctrl Pts',(6.7805179762894,0.0217759129571612,2.51834494637949));
#8464=CARTESIAN_POINT('Ctrl Pts',(6.81611962546049,-0.155110783437508,2.55325894844757));
#8465=CARTESIAN_POINT('Ctrl Pts',(6.93559514558806,-0.335467183812974,2.59501419582854));
#8466=CARTESIAN_POINT('Ctrl Pts',(7.19838636703693,-0.444497554803198,2.64699296075227));
#8467=CARTESIAN_POINT('Ctrl Pts',(7.51396784981042,-0.313675439428632,2.70919005501935));
#8468=CARTESIAN_POINT('Ctrl Pts',(7.62212313812957,-0.0514208051434247,
2.76101600110827));
#8469=CARTESIAN_POINT('Ctrl Pts',(7.57941022831611,0.159498854704775,2.80255943176652));
#8470=CARTESIAN_POINT('Ctrl Pts',(7.49002790476542,0.293811387305209,2.83377939972915));
#8471=CARTESIAN_POINT('Ctrl Pts',(7.3552499441484,0.383795703607156,2.86508254302445));
#8472=CARTESIAN_POINT('Ctrl Pts',(7.19595280633545,0.41560735445773,2.89648910888395));
#8473=CARTESIAN_POINT('Ctrl Pts',(7.03593949389396,0.383792650446306,2.92801879141503));
#8474=CARTESIAN_POINT('Ctrl Pts',(6.89961651509014,0.292876470296345,2.95969053299985));
#8475=CARTESIAN_POINT('Ctrl Pts',(6.8081238548802,0.155952445855146,2.99152250722056));
#8476=CARTESIAN_POINT('Ctrl Pts',(6.7719951154116,-0.0244720795860329,3.02708849903104));
#8477=CARTESIAN_POINT('Ctrl Pts',(6.82508694038131,-0.224423780156864,3.0664872528009));
#8478=CARTESIAN_POINT('Ctrl Pts',(6.9861130399098,-0.385566648672682,3.1098474493302));
#8479=CARTESIAN_POINT('Ctrl Pts',(7.18949761386412,-0.440411898981026,3.14997109794484));
#8480=CARTESIAN_POINT('Ctrl Pts',(7.37626527013998,-0.403213775048244,3.18676673081186));
#8481=CARTESIAN_POINT('Ctrl Pts',(7.51993103796524,-0.30750405465344,3.2201390303787));
#8482=CARTESIAN_POINT('Ctrl Pts',(7.61665044076158,-0.16281791922389,3.25377599756719));
#8483=CARTESIAN_POINT('Ctrl Pts',(7.65498225700094,0.0283123086785322,3.29145196922942));
#8484=CARTESIAN_POINT('Ctrl Pts',(7.59852316170633,0.240631420079613,3.3332902111484));
#8485=CARTESIAN_POINT('Ctrl Pts',(7.42736589163809,0.412328652603764,3.37943210760514));
#8486=CARTESIAN_POINT('Ctrl Pts',(7.19081184831391,0.475941162716025,3.42607713455886));
#8487=CARTESIAN_POINT('Ctrl Pts',(6.95151342469985,0.412204069493947,3.47322302929114));
#8488=CARTESIAN_POINT('Ctrl Pts',(6.77437422620912,0.235528496642651,3.52086247665056));
#8489=CARTESIAN_POINT('Ctrl Pts',(6.70856719057301,-0.00853695568196444,
3.56898306053165));
#8490=CARTESIAN_POINT('Ctrl Pts',(6.77444746404088,-0.255049338492359,3.61756749823055));
#8491=CARTESIAN_POINT('Ctrl Pts',(6.9562898685306,-0.437346140614658,3.66659366870206));
#8492=CARTESIAN_POINT('Ctrl Pts',(7.20705837195632,-0.504822359013845,3.71603499825878));
#8493=CARTESIAN_POINT('Ctrl Pts',(7.45987118758895,-0.437340247483335,3.76586064283255));
#8494=CARTESIAN_POINT('Ctrl Pts',(7.64643847266503,-0.251145802482984,3.81603581337119));
#8495=CARTESIAN_POINT('Ctrl Pts',(7.70939130979041,-0.0164226811455054,
3.86231497498143));
#8496=CARTESIAN_POINT('Ctrl Pts',(7.66665300702434,0.198091300428752,3.90458351454994));
#8497=CARTESIAN_POINT('Ctrl Pts',(7.55703831361006,0.362363180751678,3.94275824199772));
#8498=CARTESIAN_POINT('Ctrl Pts',(7.39231161872226,0.472405147713809,3.98104671473859));
#8499=CARTESIAN_POINT('Ctrl Pts',(7.19757748614764,0.511253819560404,4.01942894411337));
#8500=CARTESIAN_POINT('Ctrl Pts',(7.00243742159468,0.472394913482402,4.05788442705078));
#8501=CARTESIAN_POINT('Ctrl Pts',(6.83675859423202,0.361776141956741,4.09639221672569));
#8502=CARTESIAN_POINT('Ctrl Pts',(6.72593678453896,0.195994806221917,4.13493108529455));
#8503=CARTESIAN_POINT('Ctrl Pts',(6.6870196897812,0.000372767277272366,
4.17347960299015));
#8504=CARTESIAN_POINT('Ctrl Pts',(6.72599808190112,-0.19515902350661,4.21201632288769));
#8505=CARTESIAN_POINT('Ctrl Pts',(6.83662574734572,-0.360840864201945,4.25051978478148));
#8506=CARTESIAN_POINT('Ctrl Pts',(7.00208504736442,-0.47127212461887,4.28896891774833));
#8507=CARTESIAN_POINT('Ctrl Pts',(7.19679737636779,-0.510060779189973,4.32734248506513));
#8508=CARTESIAN_POINT('Ctrl Pts',(7.39100313831524,-0.471299286801184,4.36562087591661));
#8509=CARTESIAN_POINT('Ctrl Pts',(7.5551719819179,-0.361667391724164,4.40378216412631));
#8510=CARTESIAN_POINT('Ctrl Pts',(7.66435033350436,-0.197951056928272,4.44181269280615));
#8511=CARTESIAN_POINT('Ctrl Pts',(7.68982126235038,-0.0699660743691742,
4.46705762798012));
#8512=CARTESIAN_POINT('Ctrl Pts',(7.68982990724746,-0.00583191542195246,
4.4796574990714));
#8513=CARTESIAN_POINT('Origin',(7.65,-6.66133814775094E-16,4.45));
#8514=CARTESIAN_POINT('Origin',(7.65,-6.66133814775094E-16,4.45));
#8515=CARTESIAN_POINT('Origin',(7.65,-1.95245324213388E-18,0.55));
#8516=CARTESIAN_POINT('',(0.,0.,0.));
#8517=CARTESIAN_POINT('Origin',(0.,0.,0.));
#8518=CARTESIAN_POINT('',(-0.32,0.16,3.91886975727153E-17));
#8519=CARTESIAN_POINT('Origin',(0.,0.16,0.));
#8520=CARTESIAN_POINT('',(-0.32,0.,3.91886975727153E-17));
#8521=CARTESIAN_POINT('',(-0.32,0.,3.91886975727153E-17));
#8522=CARTESIAN_POINT('Origin',(0.,0.,0.));
#8523=CARTESIAN_POINT('Origin',(0.,0.,0.));
#8524=CARTESIAN_POINT('',(-0.6,0.16,7.34788079488412E-17));
#8525=CARTESIAN_POINT('Origin',(0.,0.16,0.));
#8526=CARTESIAN_POINT('',(-0.6,0.,7.34788079488412E-17));
#8527=CARTESIAN_POINT('',(-0.6,0.,7.34788079488412E-17));
#8528=CARTESIAN_POINT('Origin',(0.,0.,0.));
#8529=CARTESIAN_POINT('Origin',(0.,0.16,0.));
#8530=CARTESIAN_POINT('Origin',(0.,0.,0.));
#8531=CARTESIAN_POINT('',(0.,0.,0.));
#8532=CARTESIAN_POINT('Origin',(0.144337567297406,-0.6,-0.25));
#8533=CARTESIAN_POINT('',(0.288675134594813,-0.6,0.));
#8534=CARTESIAN_POINT('',(0.144337567297406,-0.6,-0.25));
#8535=CARTESIAN_POINT('',(0.288675134594813,-0.6,0.));
#8536=CARTESIAN_POINT('',(0.144337567297406,-0.96,-0.25));
#8537=CARTESIAN_POINT('',(0.144337567297406,-0.6,-0.25));
#8538=CARTESIAN_POINT('',(0.288675134594813,-0.96,0.));
#8539=CARTESIAN_POINT('',(0.288675134594813,-0.96,0.));
#8540=CARTESIAN_POINT('',(0.288675134594813,-0.6,0.));
#8541=CARTESIAN_POINT('Origin',(-0.144337567297406,-0.6,-0.25));
#8542=CARTESIAN_POINT('',(-0.144337567297406,-0.6,-0.25));
#8543=CARTESIAN_POINT('',(0.144337567297406,-0.6,-0.25));
#8544=CARTESIAN_POINT('',(-0.144337567297406,-0.96,-0.25));
#8545=CARTESIAN_POINT('',(-0.144337567297406,-0.6,-0.25));
#8546=CARTESIAN_POINT('',(0.144337567297406,-0.96,-0.25));
#8547=CARTESIAN_POINT('Origin',(-0.288675134594813,-0.6,-8.32667268468867E-17));
#8548=CARTESIAN_POINT('',(-0.288675134594813,-0.6,-3.53525079574969E-17));
#8549=CARTESIAN_POINT('',(-0.144337567297406,-0.6,-0.25));
#8550=CARTESIAN_POINT('',(-0.288675134594813,-0.96,-5.55111512312578E-17));
#8551=CARTESIAN_POINT('',(-0.288675134594813,-0.6,-3.53525079574969E-17));
#8552=CARTESIAN_POINT('',(-0.144337567297406,-0.96,-0.25));
#8553=CARTESIAN_POINT('Origin',(-0.144337567297407,-0.6,0.25));
#8554=CARTESIAN_POINT('',(-0.144337567297407,-0.6,0.25));
#8555=CARTESIAN_POINT('',(-0.288675134594813,-0.6,-3.53525079574969E-17));
#8556=CARTESIAN_POINT('',(-0.144337567297407,-0.96,0.25));
#8557=CARTESIAN_POINT('',(-0.144337567297407,-0.6,0.25));
#8558=CARTESIAN_POINT('',(-0.288675134594813,-0.96,-3.53525079574969E-17));
#8559=CARTESIAN_POINT('Origin',(0.144337567297406,-0.6,0.25));
#8560=CARTESIAN_POINT('',(0.144337567297406,-0.6,0.25));
#8561=CARTESIAN_POINT('',(-0.144337567297407,-0.6,0.25));
#8562=CARTESIAN_POINT('',(0.144337567297406,-0.96,0.25));
#8563=CARTESIAN_POINT('',(0.144337567297406,-0.6,0.25));
#8564=CARTESIAN_POINT('',(-0.144337567297407,-0.96,0.25));
#8565=CARTESIAN_POINT('Origin',(0.288675134594813,-0.6,0.));
#8566=CARTESIAN_POINT('',(0.144337567297406,-0.6,0.25));
#8567=CARTESIAN_POINT('',(0.144337567297406,-0.96,0.25));
#8568=CARTESIAN_POINT('Origin',(0.,-0.6,0.));
#8569=CARTESIAN_POINT('Origin',(0.,-0.96,0.));
#8570=CARTESIAN_POINT('Origin',(0.,-1.8,0.));
#8571=CARTESIAN_POINT('',(-0.2942,-1.8,3.60291088309151E-17));
#8572=CARTESIAN_POINT('Origin',(0.,-1.8,0.));
#8573=CARTESIAN_POINT('Origin',(0.45,0.6,0.));
#8574=CARTESIAN_POINT('',(-0.45,0.6,-5.51091059616309E-17));
#8575=CARTESIAN_POINT('Origin',(0.,0.6,0.));
#8576=CARTESIAN_POINT('Origin',(0.,0.575,0.));
#8577=CARTESIAN_POINT('',(-0.5,0.55,-6.12323399573677E-17));
#8578=CARTESIAN_POINT('Origin',(0.,0.55,0.));
#8579=CARTESIAN_POINT('',(-0.475,0.575,-5.81707229594993E-17));
#8580=CARTESIAN_POINT('Origin',(0.,0.29,0.));
#8581=CARTESIAN_POINT('',(-0.5,0.0299999999999998,-6.12323399573677E-17));
#8582=CARTESIAN_POINT('Origin',(0.,0.0299999999999998,0.));
#8583=CARTESIAN_POINT('',(-0.5,0.29,-6.12323399573677E-17));
#8584=CARTESIAN_POINT('Origin',(0.,0.0150000000000001,0.));
#8585=CARTESIAN_POINT('',(-0.47,7.11236625150491E-17,-5.75583995599256E-17));
#8586=CARTESIAN_POINT('Origin',(0.,0.,0.));
#8587=CARTESIAN_POINT('',(-0.485,0.0150000000000001,-5.93953697586466E-17));
#8588=CARTESIAN_POINT('Origin',(0.32,0.,0.));
#8589=CARTESIAN_POINT('',(-0.32,-6.93889390390723E-18,-3.91886975727153E-17));
#8590=CARTESIAN_POINT('Origin',(0.,0.,0.));
#8591=CARTESIAN_POINT('Origin',(0.,-0.02,0.));
#8592=CARTESIAN_POINT('',(-0.2942,-0.0515999999999999,3.60291088309151E-17));
#8593=CARTESIAN_POINT('Origin',(0.,-0.0515999999999999,0.));
#8594=CARTESIAN_POINT('',(-0.31,-0.02,-3.7964050773568E-17));
#8595=CARTESIAN_POINT('Origin',(0.,-1.24,0.));
#8596=CARTESIAN_POINT('',(-0.2942,-1.24,-3.60291088309151E-17));
#8597=CARTESIAN_POINT('',(0.,0.,0.));
#8598=CARTESIAN_POINT('',(0.,0.,0.));
#8599=CARTESIAN_POINT('Origin',(0.,0.,0.));
#8600=CARTESIAN_POINT('',(-1.88531,-0.410863395882378,-2.3088388569005E-16));
#8601=CARTESIAN_POINT('',(-2.3088388569005E-16,-0.410863395882378,1.88531));
#8602=CARTESIAN_POINT('Origin',(0.,-0.410863395882378,0.));
#8603=CARTESIAN_POINT('Origin',(0.,-0.410863395882378,0.));
#8604=CARTESIAN_POINT('',(-2.3088388569005E-16,0.410863395882378,1.88531));
#8605=CARTESIAN_POINT('Origin',(-2.35744508835865E-16,0.,1.925));
#8606=CARTESIAN_POINT('',(-1.88531,0.410863395882378,2.3088388569005E-16));
#8607=CARTESIAN_POINT('Origin',(0.,0.410863395882378,0.));
#8608=CARTESIAN_POINT('Origin',(0.,0.410863395882378,0.));
#8609=CARTESIAN_POINT('Origin',(0.,0.,0.));
#8610=CARTESIAN_POINT('',(-1.88531,0.75,-2.3088388569005E-16));
#8611=CARTESIAN_POINT('',(-1.88531,0.,-2.3088388569005E-16));
#8612=CARTESIAN_POINT('Origin',(0.,0.75,0.));
#8613=CARTESIAN_POINT('Origin',(0.,0.,0.));
#8614=CARTESIAN_POINT('',(-1.25,-0.65,-1.53080849893419E-16));
#8615=CARTESIAN_POINT('Origin',(0.,-0.65,0.));
#8616=CARTESIAN_POINT('',(-1.25,0.65,-1.53080849893419E-16));
#8617=CARTESIAN_POINT('',(-1.25,0.,-1.53080849893419E-16));
#8618=CARTESIAN_POINT('Origin',(0.,0.65,0.));
#8619=CARTESIAN_POINT('Origin',(0.,0.7,0.));
#8620=CARTESIAN_POINT('',(-1.35,0.75,-1.65327317884893E-16));
#8621=CARTESIAN_POINT('',(-1.3,0.7,-1.59204083889156E-16));
#8622=CARTESIAN_POINT('Origin',(0.,0.75,0.));
#8623=CARTESIAN_POINT('Origin',(1.88531,0.75,0.));
#8624=CARTESIAN_POINT('Origin',(0.,0.,0.));
#8625=CARTESIAN_POINT('',(-1.88531,-0.75,-2.3088388569005E-16));
#8626=CARTESIAN_POINT('Origin',(0.,-0.75,0.));
#8627=CARTESIAN_POINT('',(-1.88531,0.,-2.3088388569005E-16));
#8628=CARTESIAN_POINT('Origin',(1.35,-0.75,0.));
#8629=CARTESIAN_POINT('',(-1.35,-0.75,-1.65327317884893E-16));
#8630=CARTESIAN_POINT('Origin',(0.,-0.75,0.));
#8631=CARTESIAN_POINT('Origin',(0.,-0.7,0.));
#8632=CARTESIAN_POINT('',(-1.3,-0.7,-1.59204083889156E-16));
#8633=CARTESIAN_POINT('',(0.,0.,0.));
#8634=CARTESIAN_POINT('Origin',(0.,0.,0.));
#8635=CARTESIAN_POINT('',(-1.96469,0.410863395882378,-2.40605131981681E-16));
#8636=CARTESIAN_POINT('',(-2.40605131981681E-16,0.410863395882378,1.96469));
#8637=CARTESIAN_POINT('Origin',(0.,0.410863395882378,0.));
#8638=CARTESIAN_POINT('Origin',(0.,0.410863395882378,0.));
#8639=CARTESIAN_POINT('',(-2.40605131981681E-16,-0.410863395882378,1.96469));
#8640=CARTESIAN_POINT('Origin',(-2.35744508835865E-16,0.,1.925));
#8641=CARTESIAN_POINT('',(-1.96469,-0.410863395882378,2.40605131981681E-16));
#8642=CARTESIAN_POINT('Origin',(0.,-0.410863395882378,0.));
#8643=CARTESIAN_POINT('Origin',(0.,-0.410863395882378,0.));
#8644=CARTESIAN_POINT('Origin',(0.,0.,0.));
#8645=CARTESIAN_POINT('',(-1.96469,-0.75,-2.40605131981681E-16));
#8646=CARTESIAN_POINT('Origin',(0.,-0.75,0.));
#8647=CARTESIAN_POINT('',(-1.96469,0.,-2.40605131981681E-16));
#8648=CARTESIAN_POINT('Origin',(2.5,0.75,0.));
#8649=CARTESIAN_POINT('',(-2.5,0.75,-3.06161699786838E-16));
#8650=CARTESIAN_POINT('Origin',(0.,0.75,0.));
#8651=CARTESIAN_POINT('',(-1.96469,0.75,-2.40605131981681E-16));
#8652=CARTESIAN_POINT('Origin',(0.,0.75,0.));
#8653=CARTESIAN_POINT('Origin',(0.,0.7,0.));
#8654=CARTESIAN_POINT('',(-2.6,0.65,-3.18408167778312E-16));
#8655=CARTESIAN_POINT('Origin',(0.,0.65,0.));
#8656=CARTESIAN_POINT('',(-2.55,0.7,-3.12284933782575E-16));
#8657=CARTESIAN_POINT('Origin',(0.,0.,0.));
#8658=CARTESIAN_POINT('',(-2.6,-0.65,-3.18408167778312E-16));
#8659=CARTESIAN_POINT('Origin',(0.,-0.65,0.));
#8660=CARTESIAN_POINT('',(-2.6,0.,-3.18408167778312E-16));
#8661=CARTESIAN_POINT('Origin',(0.,-0.7,0.));
#8662=CARTESIAN_POINT('',(-2.5,-0.75,-3.06161699786838E-16));
#8663=CARTESIAN_POINT('Origin',(0.,-0.75,0.));
#8664=CARTESIAN_POINT('',(-2.55,-0.7,-3.12284933782575E-16));
#8665=CARTESIAN_POINT('Origin',(1.96469,-0.75,0.));
#8666=CARTESIAN_POINT('Origin',(0.,0.,0.));
#8667=CARTESIAN_POINT('',(-1.96469,0.,-2.40605131981681E-16));
#8668=CARTESIAN_POINT('',(0.,0.,0.));
#8669=CARTESIAN_POINT('Origin',(1.925,0.,0.));
#8670=CARTESIAN_POINT('',(1.925,-2.97627328869245E-33,0.3969));
#8671=CARTESIAN_POINT('',(1.925,-2.97627328869245E-33,-0.3969));
#8672=CARTESIAN_POINT('Origin',(1.925,0.,0.));
#8673=CARTESIAN_POINT('Origin',(1.47463555300403,0.,-1.23736614864659));
#8674=CARTESIAN_POINT('',(1.72975795528862,-2.97627328869245E-33,-0.933323109172666));
#8675=CARTESIAN_POINT('',(1.21951315071945,-2.97627328869245E-33,-1.54140918812051));
#8676=CARTESIAN_POINT('Origin',(1.47463555300403,0.,-1.23736614864659));
#8677=CARTESIAN_POINT('Origin',(0.334272742008841,0.,-1.8957549245485));
#8678=CARTESIAN_POINT('',(0.725142939179386,1.05214622327121E-34,-1.8268339628325));
#8679=CARTESIAN_POINT('',(-0.0565974551617042,-6.05776119971203E-33,-1.96467588626451));
#8680=CARTESIAN_POINT('Origin',(0.334272742008841,0.,-1.8957549245485));
#8681=CARTESIAN_POINT('Origin',(-0.9625,0.,-1.66709890228504));
#8682=CARTESIAN_POINT('',(-0.618774517237956,-2.97627328869245E-33,-1.86554890228504));
#8683=CARTESIAN_POINT('',(-1.30622548276204,-2.97627328869245E-33,-1.46864890228504));
#8684=CARTESIAN_POINT('Origin',(-0.9625,0.,-1.66709890228504));
#8685=CARTESIAN_POINT('Origin',(-1.80890829501287,0.,-0.658388775901913));
#8686=CARTESIAN_POINT('',(-1.67316050012692,1.05214622327121E-34,-1.03135277709184));
#8687=CARTESIAN_POINT('',(-1.94465608989883,-6.05776119971203E-33,-0.285424774711986));
#8688=CARTESIAN_POINT('Origin',(-1.80890829501287,0.,-0.658388775901913));
#8689=CARTESIAN_POINT('Origin',(-1.80890829501287,0.,0.658388775901912));
#8690=CARTESIAN_POINT('',(-1.94465608989883,-9.13924911073161E-33,0.285424774711985));
#8691=CARTESIAN_POINT('',(-1.67316050012692,3.1867025333467E-33,1.03135277709184));
#8692=CARTESIAN_POINT('Origin',(-1.80890829501287,0.,0.658388775901912));
#8693=CARTESIAN_POINT('Origin',(-0.962500000000001,0.,1.66709890228504));
#8694=CARTESIAN_POINT('',(-1.30622548276204,-2.97627328869245E-33,1.46864890228504));
#8695=CARTESIAN_POINT('',(-0.618774517237957,-2.97627328869245E-33,1.86554890228504));
#8696=CARTESIAN_POINT('Origin',(-0.962500000000001,0.,1.66709890228504));
#8697=CARTESIAN_POINT('Origin',(0.33427274200884,0.,1.8957549245485));
#8698=CARTESIAN_POINT('',(-0.0565974551617051,-2.97627328869245E-33,1.96467588626451));
#8699=CARTESIAN_POINT('',(0.725142939179386,-2.97627328869245E-33,1.8268339628325));
#8700=CARTESIAN_POINT('Origin',(0.33427274200884,0.,1.8957549245485));
#8701=CARTESIAN_POINT('Origin',(1.47463555300403,0.,1.23736614864659));
#8702=CARTESIAN_POINT('',(1.21951315071944,-6.05776119971203E-33,1.54140918812051));
#8703=CARTESIAN_POINT('',(1.72975795528862,1.05214622327122E-34,0.933323109172667));
#8704=CARTESIAN_POINT('Origin',(1.47463555300403,0.,1.23736614864659));
#8705=CARTESIAN_POINT('',(0.,0.,0.));
#8706=CARTESIAN_POINT('Origin',(1.47463555300403,0.,1.23736614864659));
#8707=CARTESIAN_POINT('',(1.16188454446795,-0.07938,1.49479506783723));
#8708=CARTESIAN_POINT('',(1.67384490577674,-0.07938,0.884664467981643));
#8709=CARTESIAN_POINT('Ctrl Pts',(1.16188454446795,-0.07938,1.49479506783723));
#8710=CARTESIAN_POINT('Ctrl Pts',(1.16869700612251,-0.123392992551698,1.48949983100074));
#8711=CARTESIAN_POINT('Ctrl Pts',(1.18135446441955,-0.166529565724166,1.47962830891229));
#8712=CARTESIAN_POINT('Ctrl Pts',(1.21282145231718,-0.237213819614884,1.45388393800011));
#8713=CARTESIAN_POINT('Ctrl Pts',(1.22989120215288,-0.266247928944116,1.4395843844684));
#8714=CARTESIAN_POINT('Ctrl Pts',(1.26813946847809,-0.317173992396757,1.40600777299249));
#8715=CARTESIAN_POINT('Ctrl Pts',(1.28931069477441,-0.339063173951852,1.38671820696899));
#8716=CARTESIAN_POINT('Ctrl Pts',(1.33224261954459,-0.373566122196588,1.34549913552853));
#8717=CARTESIAN_POINT('Ctrl Pts',(1.35618281536764,-0.388075792674378,1.32151296077672));
#8718=CARTESIAN_POINT('Ctrl Pts',(1.40439359896051,-0.407069005705619,1.27016020894803));
#8719=CARTESIAN_POINT('Ctrl Pts',(1.42864614483643,-0.411552957311693,1.24277684810113));
#8720=CARTESIAN_POINT('Ctrl Pts',(1.4719780748558,-0.411552957311693,1.19113586482651));
#8721=CARTESIAN_POINT('Ctrl Pts',(1.49473401052622,-0.407069005705619,1.16249669890816));
#8722=CARTESIAN_POINT('Ctrl Pts',(1.53693488395083,-0.388075792674377,1.10610103367387));
#8723=CARTESIAN_POINT('Ctrl Pts',(1.55639948343386,-0.373566122196588,1.07835938768384));
#8724=CARTESIAN_POINT('Ctrl Pts',(1.58953729406031,-0.339063173951852,1.02892207867768));
#8725=CARTESIAN_POINT('Ctrl Pts',(1.60485746336717,-0.317173992396757,1.00472289289232));
#8726=CARTESIAN_POINT('Ctrl Pts',(1.63128222892223,-0.266247928944116,0.961225186280959));
#8727=CARTESIAN_POINT('Ctrl Pts',(1.64240040915267,-0.237213819614884,0.941931672888549));
#8728=CARTESIAN_POINT('Ctrl Pts',(1.66228948011831,-0.166529565724165,0.906472276148935));
#8729=CARTESIAN_POINT('Ctrl Pts',(1.66981308703787,-0.123392992551698,0.892292941263125));
#8730=CARTESIAN_POINT('Ctrl Pts',(1.67384490577674,-0.07938,0.884664467981643));
#8731=CARTESIAN_POINT('',(1.20622598189858,-0.07938,1.54074568637942));
#8732=CARTESIAN_POINT('Origin',(1.47463555300403,-0.07938,1.23736614864659));
#8733=CARTESIAN_POINT('',(1.72679724097776,-0.07938,0.920353018170519));
#8734=CARTESIAN_POINT('Ctrl Pts',(1.72679724097776,-0.0793800000000002,
0.920353018170518));
#8735=CARTESIAN_POINT('Ctrl Pts',(1.72470909046691,-0.10165971810728,0.92427087628551));
#8736=CARTESIAN_POINT('Ctrl Pts',(1.72169532435455,-0.123845306465941,0.929898398578877));
#8737=CARTESIAN_POINT('Ctrl Pts',(1.70911544962889,-0.192537547974292,0.952957916220029));
#8738=CARTESIAN_POINT('Ctrl Pts',(1.69580594901181,-0.236239311587943,0.976785804874841));
#8739=CARTESIAN_POINT('Ctrl Pts',(1.66527150643903,-0.303218781300911,1.02787962443771));
#8740=CARTESIAN_POINT('Ctrl Pts',(1.64438322958071,-0.3351607303803,1.06123747122987));
#8741=CARTESIAN_POINT('Ctrl Pts',(1.60730731395783,-0.3732673312795,1.11639170354769));
#8742=CARTESIAN_POINT('Ctrl Pts',(1.5873911192195,-0.387903357081022,1.1447096804553));
#8743=CARTESIAN_POINT('Ctrl Pts',(1.54427174765086,-0.40704475551587,1.20224605970712));
#8744=CARTESIAN_POINT('Ctrl Pts',(1.52104964294098,-0.411552957311693,1.23144933316771));
#8745=CARTESIAN_POINT('Ctrl Pts',(1.47686834938291,-0.411552957311693,1.284102548491));
#8746=CARTESIAN_POINT('Ctrl Pts',(1.45214121543005,-0.40704475551587,1.31204295246889));
#8747=CARTESIAN_POINT('Ctrl Pts',(1.40296654335764,-0.387903357081022,1.36449833130133));
#8748=CARTESIAN_POINT('Ctrl Pts',(1.37853719107178,-0.3732673312795,1.38902931937536));
#8749=CARTESIAN_POINT('Ctrl Pts',(1.330659040657,-0.3351607303803,1.43511940046341));
#8750=CARTESIAN_POINT('Ctrl Pts',(1.30143518572334,-0.303218781300911,1.4614828667669));
#8751=CARTESIAN_POINT('Ctrl Pts',(1.25641984639565,-0.236239311587943,1.50042577120361));
#8752=CARTESIAN_POINT('Ctrl Pts',(1.23526512743829,-0.192537547974292,1.51767074004259));
#8753=CARTESIAN_POINT('Ctrl Pts',(1.21474040800595,-0.123845306465941,1.53406374142061));
#8754=CARTESIAN_POINT('Ctrl Pts',(1.20972171541452,-0.10165971810728,1.53800893064485));
#8755=CARTESIAN_POINT('Ctrl Pts',(1.20622598189858,-0.0793800000000002,
1.54074568637942));
#8756=CARTESIAN_POINT('Origin',(1.47463555300403,-0.07938,1.23736614864659));
#8757=CARTESIAN_POINT('Origin',(0.,-0.27783,0.));
#8758=CARTESIAN_POINT('',(0.731211914226578,-0.07938,1.81499518621871));
#8759=CARTESIAN_POINT('Origin',(0.,-0.07938,0.));
#8760=CARTESIAN_POINT('',(-0.0663495263035324,-0.07938,1.95562678695688));
#8761=CARTESIAN_POINT('Ctrl Pts',(0.73121191422658,-0.0793800000000002,
1.81499518621871));
#8762=CARTESIAN_POINT('Ctrl Pts',(0.727093947478514,-0.10165971810728,1.81665420238109));
#8763=CARTESIAN_POINT('Ctrl Pts',(0.721167967091869,-0.123845306465941,
1.81902792304693));
#8764=CARTESIAN_POINT('Ctrl Pts',(0.696708851738065,-0.192537547974292,
1.82860635079188));
#8765=CARTESIAN_POINT('Ctrl Pts',(0.671196911157359,-0.236239311587943,
1.83830439039938));
#8766=CARTESIAN_POINT('Ctrl Pts',(0.614963696954177,-0.303218781300911,
1.85781736559878));
#8767=CARTESIAN_POINT('Ctrl Pts',(0.577520337936704,-0.3351607303803,1.86994423321609));
#8768=CARTESIAN_POINT('Ctrl Pts',(0.513666081644577,-0.3732673312795,1.88836288721748));
#8769=CARTESIAN_POINT('Ctrl Pts',(0.48020694664961,-0.387903357081022,1.89725383285802));
#8770=CARTESIAN_POINT('Ctrl Pts',(0.410191919979371,-0.40704475551587,1.91361265867928));
#8771=CARTESIAN_POINT('Ctrl Pts',(0.373631253366087,-0.411552957311693,
1.92105678285629));
#8772=CARTESIAN_POINT('Ctrl Pts',(0.305941584526154,-0.411552957311693,
1.932992297788));
#8773=CARTESIAN_POINT('Ctrl Pts',(0.269039755480681,-0.40704475551587,1.9385015936658));
#8774=CARTESIAN_POINT('Ctrl Pts',(0.197652103622503,-0.387903357081022,
1.94707587521355));
#8775=CARTESIAN_POINT('Ctrl Pts',(0.163169918867575,-0.3732673312795,1.95016481734985));
#8776=CARTESIAN_POINT('Ctrl Pts',(0.09686699474267,-0.3351607303803,1.95469638598893));
#8777=CARTESIAN_POINT('Ctrl Pts',(0.0575341135759475,-0.30321878130091,
1.95610724099344));
#8778=CARTESIAN_POINT('Ctrl Pts',(-0.00198165342826295,-0.236239311587942,
1.95700393417042));
#8779=CARTESIAN_POINT('Ctrl Pts',(-0.0292719606304177,-0.192537547974292,
1.95661635548909));
#8780=CARTESIAN_POINT('Ctrl Pts',(-0.0555320260694991,-0.123845306465941,
1.95598108775736));
#8781=CARTESIAN_POINT('Ctrl Pts',(-0.0619124863920986,-0.10165971810728,
1.95577732462505));
#8782=CARTESIAN_POINT('Ctrl Pts',(-0.0663495263035336,-0.0793800000000002,
1.95562678695688));
#8783=CARTESIAN_POINT('',(-0.606515593706441,-0.07938,1.86038093521056));
#8784=CARTESIAN_POINT('Origin',(0.,-0.07938,0.));
#8785=CARTESIAN_POINT('',(-1.30787935375538,-0.07938,1.45544837954646));
#8786=CARTESIAN_POINT('Ctrl Pts',(-0.60651559370644,-0.0793800000000002,
1.86038093521056));
#8787=CARTESIAN_POINT('Ctrl Pts',(-0.610736534284191,-0.10165971810728,
1.85900483732004));
#8788=CARTESIAN_POINT('Ctrl Pts',(-0.616801896862274,-0.123845306465941,
1.85701406607784));
#8789=CARTESIAN_POINT('Ctrl Pts',(-0.64169556093739,-0.192537547974292,
1.84862955113236));
#8790=CARTESIAN_POINT('Ctrl Pts',(-0.667472620950374,-0.236239311587943,
1.8396599211785));
#8791=CARTESIAN_POINT('Ctrl Pts',(-0.723092460895733,-0.303218781300911,
1.81846171405606));
#8792=CARTESIAN_POINT('Ctrl Pts',(-0.759570738251496,-0.3351607303803,1.80368330636526));
#8793=CARTESIAN_POINT('Ctrl Pts',(-0.820325219032771,-0.3732673312795,1.77674808914243));
#8794=CARTESIAN_POINT('Ctrl Pts',(-0.851671393163369,-0.387903357081022,
1.76205183123884));
#8795=CARTESIAN_POINT('Ctrl Pts',(-0.915821265825857,-0.40704475551587,
1.72957862721967));
#8796=CARTESIAN_POINT('Ctrl Pts',(-0.948613352107641,-0.411552957311693,
1.71178041367846));
#8797=CARTESIAN_POINT('Ctrl Pts',(-1.00813864789236,-0.411552957311693,
1.67741346813356));
#8798=CARTESIAN_POINT('Ctrl Pts',(-1.03994839610192,-0.40704475551587,1.65791379514105));
#8799=CARTESIAN_POINT('Ctrl Pts',(-1.10014595205605,-0.387903357081022,
1.61859497777538));
#8800=CARTESIAN_POINT('Ctrl Pts',(-1.12854637180642,-0.3732673312795,1.59879652361863));
#8801=CARTESIAN_POINT('Ctrl Pts',(-1.18225019456848,-0.3351607303803,1.55964920847973));
#8802=CARTESIAN_POINT('Ctrl Pts',(-1.21328780973407,-0.30321878130091,1.53544729744874));
#8803=CARTESIAN_POINT('Ctrl Pts',(-1.25945591558947,-0.236239311587942,
1.49787820666285));
#8804=CARTESIAN_POINT('Ctrl Pts',(-1.28011237299855,-0.192537547974292,
1.48003943283366));
#8805=CARTESIAN_POINT('Ctrl Pts',(-1.29982040797731,-0.12384530646594,1.46267314482408));
#8806=CARTESIAN_POINT('Ctrl Pts',(-1.30457714773522,-0.10165971810728,1.45841577236939));
#8807=CARTESIAN_POINT('Ctrl Pts',(-1.30787935375538,-0.0793800000000002,
1.45544837954646));
#8808=CARTESIAN_POINT('',(-1.66044771467423,-0.07938,1.03527376878636));
#8809=CARTESIAN_POINT('Origin',(0.,-0.07938,0.));
#8810=CARTESIAN_POINT('',(-1.93743789612516,-0.07938,0.274249499839291));
#8811=CARTESIAN_POINT('Ctrl Pts',(-1.66044771467423,-0.0793800000000002,
1.03527376878636));
#8812=CARTESIAN_POINT('Ctrl Pts',(-1.66279660407481,-0.10165971810728,1.03150644833954));
#8813=CARTESIAN_POINT('Ctrl Pts',(-1.66616329828505,-0.123845306465941,
1.02608268917849));
#8814=CARTESIAN_POINT('Ctrl Pts',(-1.67984348899847,-0.192537547974292,
1.00365843926907));
#8815=CARTESIAN_POINT('Ctrl Pts',(-1.69382429558355,-0.236239311587943,
0.980218129295584));
#8816=CARTESIAN_POINT('Ctrl Pts',(-1.72280562001498,-0.303218781300911,
0.928227616555729));
#8817=CARTESIAN_POINT('Ctrl Pts',(-1.74125022432338,-0.3351607303803,0.893458914759057));
#8818=CARTESIAN_POINT('Ctrl Pts',(-1.7704772328254,-0.3732673312795,0.833773113802161));
#8819=CARTESIAN_POINT('Ctrl Pts',(-1.785043222842,-0.387903357081022,0.802366194758251));
#8820=CARTESIAN_POINT('Ctrl Pts',(-1.81331150313154,-0.407044755515871,
0.736255533958675));
#8821=CARTESIAN_POINT('Ctrl Pts',(-1.82699122746714,-0.411552957311693,
0.701542964620283));
#8822=CARTESIAN_POINT('Ctrl Pts',(-1.850499602749,-0.411552957311693,0.636954234365294));
#8823=CARTESIAN_POINT('Ctrl Pts',(-1.86233313540942,-0.40704475551587,0.60156970621039));
#8824=CARTESIAN_POINT('Ctrl Pts',(-1.88317349000725,-0.387903357081022,
0.53275550155669));
#8825=CARTESIAN_POINT('Ctrl Pts',(-1.89220327271636,-0.3732673312795,0.499333567842125));
#8826=CARTESIAN_POINT('Ctrl Pts',(-1.9081793785937,-0.3351607303803,0.434824832752687));
#8827=CARTESIAN_POINT('Ctrl Pts',(-1.91639888267751,-0.30321878130091,0.396334498831876));
#8828=CARTESIAN_POINT('Ctrl Pts',(-1.92761675755301,-0.236239311587942,
0.337878619195771));
#8829=CARTESIAN_POINT('Ctrl Pts',(-1.93197397917636,-0.192537547974292,
0.310935610749289));
#8830=CARTESIAN_POINT('Ctrl Pts',(-1.93590837509782,-0.12384530646594,0.284964181626328));
#8831=CARTESIAN_POINT('Ctrl Pts',(-1.93681566289304,-0.10165971810728,0.278645271736243));
#8832=CARTESIAN_POINT('Ctrl Pts',(-1.93743789612516,-0.0793800000000002,
0.27424949983929));
#8833=CARTESIAN_POINT('',(-1.956752,-0.07938,2.39633007352518E-16));
#8834=CARTESIAN_POINT('Origin',(0.,-0.07938,0.));
#8835=CARTESIAN_POINT('',(-1.956752,-0.47628,2.39633007352518E-16));
#8836=CARTESIAN_POINT('',(-1.956752,-0.27783,2.39633007352518E-16));
#8837=CARTESIAN_POINT('Origin',(0.,-0.47628,0.));
#8838=CARTESIAN_POINT('',(-1.93743789612516,-0.07938,-0.274249499839292));
#8839=CARTESIAN_POINT('Origin',(0.,-0.07938,0.));
#8840=CARTESIAN_POINT('',(-1.66044771467423,-0.07938,-1.03527376878636));
#8841=CARTESIAN_POINT('Ctrl Pts',(-1.93743789612516,-0.0793800000000002,
-0.27424949983929));
#8842=CARTESIAN_POINT('Ctrl Pts',(-1.93681566289304,-0.10165971810728,-0.278645271736244));
#8843=CARTESIAN_POINT('Ctrl Pts',(-1.93590837509782,-0.123845306465941,
-0.284964181626328));
#8844=CARTESIAN_POINT('Ctrl Pts',(-1.93197397917636,-0.192537547974292,
-0.310935610749289));
#8845=CARTESIAN_POINT('Ctrl Pts',(-1.92761675755301,-0.236239311587942,
-0.337878619195772));
#8846=CARTESIAN_POINT('Ctrl Pts',(-1.91639888267751,-0.303218781300911,
-0.396334498831877));
#8847=CARTESIAN_POINT('Ctrl Pts',(-1.9081793785937,-0.3351607303803,-0.434824832752687));
#8848=CARTESIAN_POINT('Ctrl Pts',(-1.89220327271636,-0.3732673312795,-0.499333567842125));
#8849=CARTESIAN_POINT('Ctrl Pts',(-1.88317349000725,-0.387903357081022,
-0.53275550155669));
#8850=CARTESIAN_POINT('Ctrl Pts',(-1.86233313540942,-0.40704475551587,-0.601569706210391));
#8851=CARTESIAN_POINT('Ctrl Pts',(-1.850499602749,-0.411552957311693,-0.636954234365295));
#8852=CARTESIAN_POINT('Ctrl Pts',(-1.82699122746714,-0.411552957311693,
-0.701542964620284));
#8853=CARTESIAN_POINT('Ctrl Pts',(-1.81331150313154,-0.40704475551587,-0.736255533958675));
#8854=CARTESIAN_POINT('Ctrl Pts',(-1.785043222842,-0.387903357081022,-0.802366194758251));
#8855=CARTESIAN_POINT('Ctrl Pts',(-1.7704772328254,-0.3732673312795,-0.833773113802161));
#8856=CARTESIAN_POINT('Ctrl Pts',(-1.74125022432338,-0.3351607303803,-0.893458914759057));
#8857=CARTESIAN_POINT('Ctrl Pts',(-1.72280562001498,-0.303218781300911,
-0.92822761655573));
#8858=CARTESIAN_POINT('Ctrl Pts',(-1.69382429558355,-0.236239311587942,
-0.980218129295584));
#8859=CARTESIAN_POINT('Ctrl Pts',(-1.67984348899847,-0.192537547974292,
-1.00365843926907));
#8860=CARTESIAN_POINT('Ctrl Pts',(-1.66616329828505,-0.123845306465941,
-1.02608268917849));
#8861=CARTESIAN_POINT('Ctrl Pts',(-1.66279660407481,-0.10165971810728,-1.03150644833954));
#8862=CARTESIAN_POINT('Ctrl Pts',(-1.66044771467423,-0.0793800000000001,
-1.03527376878636));
#8863=CARTESIAN_POINT('',(-1.30787935375538,-0.07938,-1.45544837954646));
#8864=CARTESIAN_POINT('Origin',(0.,-0.07938,0.));
#8865=CARTESIAN_POINT('',(-0.60651559370644,-0.07938,-1.86038093521056));
#8866=CARTESIAN_POINT('Ctrl Pts',(-1.30787935375538,-0.0793800000000002,
-1.45544837954646));
#8867=CARTESIAN_POINT('Ctrl Pts',(-1.30457714773522,-0.10165971810728,-1.45841577236939));
#8868=CARTESIAN_POINT('Ctrl Pts',(-1.29982040797731,-0.123845306465941,
-1.46267314482408));
#8869=CARTESIAN_POINT('Ctrl Pts',(-1.28011237299855,-0.192537547974292,
-1.48003943283366));
#8870=CARTESIAN_POINT('Ctrl Pts',(-1.25945591558947,-0.236239311587942,
-1.49787820666285));
#8871=CARTESIAN_POINT('Ctrl Pts',(-1.21328780973407,-0.303218781300911,
-1.53544729744874));
#8872=CARTESIAN_POINT('Ctrl Pts',(-1.18225019456848,-0.3351607303803,-1.55964920847973));
#8873=CARTESIAN_POINT('Ctrl Pts',(-1.12854637180642,-0.3732673312795,-1.59879652361863));
#8874=CARTESIAN_POINT('Ctrl Pts',(-1.10014595205605,-0.387903357081022,
-1.61859497777538));
#8875=CARTESIAN_POINT('Ctrl Pts',(-1.03994839610192,-0.40704475551587,-1.65791379514105));
#8876=CARTESIAN_POINT('Ctrl Pts',(-1.00813864789236,-0.411552957311693,
-1.67741346813356));
#8877=CARTESIAN_POINT('Ctrl Pts',(-0.948613352107639,-0.411552957311693,
-1.71178041367846));
#8878=CARTESIAN_POINT('Ctrl Pts',(-0.915821265825855,-0.40704475551587,
-1.72957862721967));
#8879=CARTESIAN_POINT('Ctrl Pts',(-0.851671393163367,-0.387903357081022,
-1.76205183123885));
#8880=CARTESIAN_POINT('Ctrl Pts',(-0.820325219032769,-0.3732673312795,-1.77674808914243));
#8881=CARTESIAN_POINT('Ctrl Pts',(-0.759570738251494,-0.3351607303803,-1.80368330636526));
#8882=CARTESIAN_POINT('Ctrl Pts',(-0.723092460895731,-0.303218781300911,
-1.81846171405606));
#8883=CARTESIAN_POINT('Ctrl Pts',(-0.667472620950373,-0.236239311587942,
-1.8396599211785));
#8884=CARTESIAN_POINT('Ctrl Pts',(-0.641695560937389,-0.192537547974292,
-1.84862955113236));
#8885=CARTESIAN_POINT('Ctrl Pts',(-0.616801896862272,-0.123845306465941,
-1.85701406607784));
#8886=CARTESIAN_POINT('Ctrl Pts',(-0.610736534284189,-0.10165971810728,
-1.85900483732004));
#8887=CARTESIAN_POINT('Ctrl Pts',(-0.606515593706439,-0.0793800000000002,
-1.86038093521056));
#8888=CARTESIAN_POINT('',(-0.0663495263035315,-0.07938,-1.95562678695688));
#8889=CARTESIAN_POINT('Origin',(0.,-0.07938,0.));
#8890=CARTESIAN_POINT('',(0.731211914226579,-0.07938,-1.81499518621871));
#8891=CARTESIAN_POINT('Ctrl Pts',(-0.0663495263035327,-0.0793800000000002,
-1.95562678695688));
#8892=CARTESIAN_POINT('Ctrl Pts',(-0.0619124863920977,-0.10165971810728,
-1.95577732462505));
#8893=CARTESIAN_POINT('Ctrl Pts',(-0.0555320260694982,-0.123845306465941,
-1.95598108775736));
#8894=CARTESIAN_POINT('Ctrl Pts',(-0.0292719606304167,-0.192537547974292,
-1.95661635548909));
#8895=CARTESIAN_POINT('Ctrl Pts',(-0.00198165342826177,-0.236239311587943,
-1.95700393417042));
#8896=CARTESIAN_POINT('Ctrl Pts',(0.0575341135759488,-0.303218781300911,
-1.95610724099344));
#8897=CARTESIAN_POINT('Ctrl Pts',(0.0968669947426714,-0.3351607303803,-1.95469638598893));
#8898=CARTESIAN_POINT('Ctrl Pts',(0.163169918867576,-0.3732673312795,-1.95016481734985));
#8899=CARTESIAN_POINT('Ctrl Pts',(0.197652103622504,-0.387903357081022,
-1.94707587521355));
#8900=CARTESIAN_POINT('Ctrl Pts',(0.269039755480682,-0.40704475551587,-1.9385015936658));
#8901=CARTESIAN_POINT('Ctrl Pts',(0.305941584526155,-0.411552957311693,
-1.93299229778799));
#8902=CARTESIAN_POINT('Ctrl Pts',(0.373631253366089,-0.411552957311693,
-1.92105678285629));
#8903=CARTESIAN_POINT('Ctrl Pts',(0.410191919979372,-0.40704475551587,-1.91361265867928));
#8904=CARTESIAN_POINT('Ctrl Pts',(0.480206946649611,-0.387903357081022,
-1.89725383285802));
#8905=CARTESIAN_POINT('Ctrl Pts',(0.513666081644578,-0.3732673312795,-1.88836288721748));
#8906=CARTESIAN_POINT('Ctrl Pts',(0.577520337936705,-0.3351607303803,-1.86994423321609));
#8907=CARTESIAN_POINT('Ctrl Pts',(0.614963696954178,-0.30321878130091,-1.85781736559878));
#8908=CARTESIAN_POINT('Ctrl Pts',(0.67119691115736,-0.236239311587942,-1.83830439039938));
#8909=CARTESIAN_POINT('Ctrl Pts',(0.696708851738067,-0.192537547974292,
-1.82860635079188));
#8910=CARTESIAN_POINT('Ctrl Pts',(0.721167967091869,-0.123845306465941,
-1.81902792304693));
#8911=CARTESIAN_POINT('Ctrl Pts',(0.727093947478515,-0.10165971810728,-1.81665420238109));
#8912=CARTESIAN_POINT('Ctrl Pts',(0.73121191422658,-0.0793800000000002,
-1.81499518621871));
#8913=CARTESIAN_POINT('',(1.20622598189858,-0.07938,-1.54074568637942));
#8914=CARTESIAN_POINT('Origin',(0.,-0.07938,0.));
#8915=CARTESIAN_POINT('',(1.72679724097776,-0.07938,-0.920353018170518));
#8916=CARTESIAN_POINT('Ctrl Pts',(1.20622598189858,-0.0793800000000002,
-1.54074568637942));
#8917=CARTESIAN_POINT('Ctrl Pts',(1.20972171541452,-0.10165971810728,-1.53800893064485));
#8918=CARTESIAN_POINT('Ctrl Pts',(1.21474040800596,-0.123845306465941,-1.53406374142061));
#8919=CARTESIAN_POINT('Ctrl Pts',(1.23526512743829,-0.192537547974292,-1.51767074004259));
#8920=CARTESIAN_POINT('Ctrl Pts',(1.25641984639565,-0.236239311587942,-1.50042577120361));
#8921=CARTESIAN_POINT('Ctrl Pts',(1.30143518572334,-0.303218781300911,-1.4614828667669));
#8922=CARTESIAN_POINT('Ctrl Pts',(1.330659040657,-0.3351607303803,-1.43511940046341));
#8923=CARTESIAN_POINT('Ctrl Pts',(1.37853719107178,-0.3732673312795,-1.38902931937536));
#8924=CARTESIAN_POINT('Ctrl Pts',(1.40296654335764,-0.387903357081022,-1.36449833130133));
#8925=CARTESIAN_POINT('Ctrl Pts',(1.45214121543005,-0.40704475551587,-1.31204295246889));
#8926=CARTESIAN_POINT('Ctrl Pts',(1.47686834938291,-0.411552957311693,-1.284102548491));
#8927=CARTESIAN_POINT('Ctrl Pts',(1.52104964294098,-0.411552957311693,-1.23144933316771));
#8928=CARTESIAN_POINT('Ctrl Pts',(1.54427174765086,-0.407044755515871,-1.20224605970712));
#8929=CARTESIAN_POINT('Ctrl Pts',(1.5873911192195,-0.387903357081022,-1.1447096804553));
#8930=CARTESIAN_POINT('Ctrl Pts',(1.60730731395783,-0.3732673312795,-1.11639170354769));
#8931=CARTESIAN_POINT('Ctrl Pts',(1.64438322958071,-0.3351607303803,-1.06123747122987));
#8932=CARTESIAN_POINT('Ctrl Pts',(1.66527150643903,-0.303218781300911,-1.02787962443771));
#8933=CARTESIAN_POINT('Ctrl Pts',(1.69580594901181,-0.236239311587943,-0.976785804874841));
#8934=CARTESIAN_POINT('Ctrl Pts',(1.70911544962889,-0.192537547974292,-0.952957916220028));
#8935=CARTESIAN_POINT('Ctrl Pts',(1.72169532435455,-0.123845306465941,-0.929898398578876));
#8936=CARTESIAN_POINT('Ctrl Pts',(1.72470909046691,-0.10165971810728,-0.924270876285509));
#8937=CARTESIAN_POINT('Ctrl Pts',(1.72679724097776,-0.0793800000000002,
-0.920353018170518));
#8938=CARTESIAN_POINT('',(1.91439494746182,-0.07938,-0.404932555664102));
#8939=CARTESIAN_POINT('Origin',(0.,-0.07938,0.));
#8940=CARTESIAN_POINT('',(1.91439494746182,-0.07938,0.404932555664102));
#8941=CARTESIAN_POINT('Ctrl Pts',(1.91439494746182,-0.0793800000000002,
-0.404932555664103));
#8942=CARTESIAN_POINT('Ctrl Pts',(1.91531368201941,-0.10165971810728,-0.400589064950645));
#8943=CARTESIAN_POINT('Ctrl Pts',(1.91662230483958,-0.123845306465941,-0.394340921253764));
#8944=CARTESIAN_POINT('Ctrl Pts',(1.92180793393594,-0.192537547974292,-0.368590118298695));
#8945=CARTESIAN_POINT('Ctrl Pts',(1.92692853653984,-0.236239311587943,-0.341781714515643));
#8946=CARTESIAN_POINT('Ctrl Pts',(1.9363802706298,-0.303218781300911,-0.283014416607319));
#8947=CARTESIAN_POINT('Ctrl Pts',(1.94182093281998,-0.3351607303803,-0.244034097885537));
#8948=CARTESIAN_POINT('Ctrl Pts',(1.94887159083919,-0.3732673312795,-0.177951565523803));
#8949=CARTESIAN_POINT('Ctrl Pts',(1.95181734521941,-0.387903357081022,-0.143456853463462));
#8950=CARTESIAN_POINT('Ctrl Pts',(1.95576966192778,-0.40704475551587,-0.071664832078622));
#8951=CARTESIAN_POINT('Ctrl Pts',(1.956752,-0.411552957311693,-0.0343669455449008));
#8952=CARTESIAN_POINT('Ctrl Pts',(1.956752,-0.411552957311693,0.0343669455449008));
#8953=CARTESIAN_POINT('Ctrl Pts',(1.95576966192778,-0.40704475551587,0.0716648320786219));
#8954=CARTESIAN_POINT('Ctrl Pts',(1.95181734521941,-0.387903357081022,0.143456853463462));
#8955=CARTESIAN_POINT('Ctrl Pts',(1.94887159083919,-0.3732673312795,0.177951565523803));
#8956=CARTESIAN_POINT('Ctrl Pts',(1.94182093281998,-0.3351607303803,0.244034097885537));
#8957=CARTESIAN_POINT('Ctrl Pts',(1.9363802706298,-0.303218781300911,0.283014416607319));
#8958=CARTESIAN_POINT('Ctrl Pts',(1.92692853653984,-0.236239311587943,0.341781714515643));
#8959=CARTESIAN_POINT('Ctrl Pts',(1.92180793393594,-0.192537547974292,0.368590118298695));
#8960=CARTESIAN_POINT('Ctrl Pts',(1.91662230483958,-0.123845306465941,0.394340921253764));
#8961=CARTESIAN_POINT('Ctrl Pts',(1.91531368201941,-0.10165971810728,0.400589064950645));
#8962=CARTESIAN_POINT('Ctrl Pts',(1.91439494746182,-0.0793800000000002,
0.404932555664103));
#8963=CARTESIAN_POINT('Origin',(0.,-0.07938,0.));
#8964=CARTESIAN_POINT('Origin',(0.,-0.07938,0.));
#8965=CARTESIAN_POINT('',(0.71358822996475,-0.07938,1.75361906569237));
#8966=CARTESIAN_POINT('Origin',(0.,-0.07938,0.));
#8967=CARTESIAN_POINT('Origin',(0.33427274200884,-0.07938,1.8957549245485));
#8968=CARTESIAN_POINT('Origin',(0.33427274200884,0.,1.8957549245485));
#8969=CARTESIAN_POINT('',(-0.070780549790825,-0.07938,1.89192444438865));
#8970=CARTESIAN_POINT('Ctrl Pts',(-0.0707805497908251,-0.07938,1.89192444438865));
#8971=CARTESIAN_POINT('Ctrl Pts',(-0.0621581887675352,-0.123392992551698,
1.89224702357808));
#8972=CARTESIAN_POINT('Ctrl Pts',(-0.0461167210878756,-0.166529565724166,
1.89282105630055));
#8973=CARTESIAN_POINT('Ctrl Pts',(-0.00546344722567869,-0.237213819614884,
1.89332631395644));
#8974=CARTESIAN_POINT('Ctrl Pts',(0.0168043156156246,-0.266247928944116,
1.89334444412923));
#8975=CARTESIAN_POINT('Ctrl Pts',(0.0676868173249578,-0.317173992396757,
1.89220877917518));
#8976=CARTESIAN_POINT('Ctrl Pts',(0.0963040116194015,-0.339063173951852,
1.89104071625784));
#8977=CARTESIAN_POINT('Ctrl Pts',(0.155686882426711,-0.373566122196588,
1.88706118493262));
#8978=CARTESIAN_POINT('Ctrl Pts',(0.189444152338378,-0.388075792674378,
1.88407517030084));
#8979=CARTESIAN_POINT('Ctrl Pts',(0.259384667806906,-0.407069005705619,
1.87572597447038));
#8980=CARTESIAN_POINT('Ctrl Pts',(0.295564880870602,-0.411552957311693,
1.87033833905209));
#8981=CARTESIAN_POINT('Ctrl Pts',(0.361953249272518,-0.411552957311693,
1.85863227849762));
#8982=CARTESIAN_POINT('Ctrl Pts',(0.397794208344885,-0.407069005705619,
1.85132063808607));
#8983=CARTESIAN_POINT('Ctrl Pts',(0.466372387779211,-0.388075792674377,
1.83524525067264));
#8984=CARTESIAN_POINT('Ctrl Pts',(0.499115122365417,-0.373566122196588,
1.82650552029421));
#8985=CARTESIAN_POINT('Ctrl Pts',(0.55627784773835,-0.339063173951852,1.8099349185301));
#8986=CARTESIAN_POINT('Ctrl Pts',(0.583568715090836,-0.317173992396757,
1.80124488173997));
#8987=CARTESIAN_POINT('Ctrl Pts',(0.631771046764577,-0.266247928944116,
1.78490921718958));
#8988=CARTESIAN_POINT('Ctrl Pts',(0.652689698303665,-0.237213819614884,
1.77727615696148));
#8989=CARTESIAN_POINT('Ctrl Pts',(0.690718471466875,-0.166529565724165,
1.76289713151763));
#8990=CARTESIAN_POINT('Ctrl Pts',(0.705596189518013,-0.123392992551698,
1.75687121212928));
#8991=CARTESIAN_POINT('Ctrl Pts',(0.71358822996475,-0.07938,1.75361906569237));
#8992=CARTESIAN_POINT('Origin',(0.33427274200884,-0.07938,1.8957549245485));
#8993=CARTESIAN_POINT('Origin',(0.,-0.07938,0.));
#8994=CARTESIAN_POINT('',(-0.580564309297537,-0.07938,1.80203581326062));
#8995=CARTESIAN_POINT('Origin',(0.,-0.07938,0.));
#8996=CARTESIAN_POINT('Origin',(-0.962500000000001,-0.07938,1.66709890228504));
#8997=CARTESIAN_POINT('Origin',(-0.962500000000001,0.,1.66709890228504));
#8998=CARTESIAN_POINT('',(-1.27032663816428,-0.07938,1.40380134701254));
#8999=CARTESIAN_POINT('Ctrl Pts',(-1.27032663816428,-0.07938,1.40380134701254));
#9000=CARTESIAN_POINT('Ctrl Pts',(-1.26392887632193,-0.123392992551698,
1.40959080384008));
#9001=CARTESIAN_POINT('Ctrl Pts',(-1.25200938026802,-0.166529565724166,
1.42034179508297));
#9002=CARTESIAN_POINT('Ctrl Pts',(-1.22119193909219,-0.237213819614885,
1.44686026563443));
#9003=CARTESIAN_POINT('Ctrl Pts',(-1.20414549695735,-0.266247928944117,
1.46118759620237));
#9004=CARTESIAN_POINT('Ctrl Pts',(-1.16443724790971,-0.317173992396758,
1.49302426802369));
#9005=CARTESIAN_POINT('Ctrl Pts',(-1.14176438887219,-0.339063173951853,
1.51052425783311));
#9006=CARTESIAN_POINT('Ctrl Pts',(-1.09371647724559,-0.373566122196589,
1.54564633355776));
#9007=CARTESIAN_POINT('Ctrl Pts',(-1.06593753500724,-0.388075792674378,
1.56505766847808));
#9008=CARTESIAN_POINT('Ctrl Pts',(-1.00699323215303,-0.407069005705619,
1.6036187101659));
#9009=CARTESIAN_POINT('Ctrl Pts',(-0.975814475692339,-0.411552957311693,
1.62274773466534));
#9010=CARTESIAN_POINT('Ctrl Pts',(-0.917433524307661,-0.411552957311693,
1.65645399266283));
#9011=CARTESIAN_POINT('Ctrl Pts',(-0.885277924911194,-0.407069005705619,
1.67389107556648));
#9012=CARTESIAN_POINT('Ctrl Pts',(-0.822410931786043,-0.388075792674377,
1.70565781840267));
#9013=CARTESIAN_POINT('Ctrl Pts',(-0.791710751504505,-0.373566122196588,
1.72000942061118));
#9014=CARTESIAN_POINT('Ctrl Pts',(-0.737270185880016,-0.339063173951852,
1.74405909481629));
#9015=CARTESIAN_POINT('Ctrl Pts',(-0.710778320620332,-0.317173992396757,
1.75494437181449));
#9016=CARTESIAN_POINT('Ctrl Pts',(-0.663352829527299,-0.266247928944116,
1.77341438831889));
#9017=CARTESIAN_POINT('Ctrl Pts',(-0.642421776219621,-0.237213819614884,
1.78101337496783));
#9018=CARTESIAN_POINT('Ctrl Pts',(-0.604047386464641,-0.166529565724165,
1.79444282663));
#9019=CARTESIAN_POINT('Ctrl Pts',(-0.588777006905475,-0.123392992551698,
1.79938991739155));
#9020=CARTESIAN_POINT('Ctrl Pts',(-0.580564309297537,-0.0793799999999999,
1.80203581326062));
#9021=CARTESIAN_POINT('Origin',(-0.962500000000001,-0.07938,1.66709890228504));
#9022=CARTESIAN_POINT('Origin',(0.,-0.07938,0.));
#9023=CARTESIAN_POINT('',(-1.60306435598592,-0.07938,1.00725997640701));
#9024=CARTESIAN_POINT('Origin',(0.,-0.07938,0.));
#9025=CARTESIAN_POINT('Origin',(-1.80890829501287,-0.07938,0.658388775901912));
#9026=CARTESIAN_POINT('Origin',(-1.80890829501287,0.,0.658388775901912));
#9027=CARTESIAN_POINT('',(-1.8754727744327,-0.07938,0.258823997855139));
#9028=CARTESIAN_POINT('Ctrl Pts',(-1.8754727744327,-0.07938,0.258823997855138));
#9029=CARTESIAN_POINT('Ctrl Pts',(-1.87429319564052,-0.123392992551698,
0.267371381128541));
#9030=CARTESIAN_POINT('Ctrl Pts',(-1.87207293588642,-0.166529565724165,
0.283268822605344));
#9031=CARTESIAN_POINT('Ctrl Pts',(-1.86551115062085,-0.237213819614884,
0.323392218961362));
#9032=CARTESIAN_POINT('Ctrl Pts',(-1.86166224891746,-0.266247928944116,
0.34532483272118));
#9033=CARTESIAN_POINT('Ctrl Pts',(-1.85170818356893,-0.317173992396757,
0.395237108747477));
#9034=CARTESIAN_POINT('Ctrl Pts',(-1.84558854251276,-0.339063173951852,
0.423216711561106));
#9035=CARTESIAN_POINT('Ctrl Pts',(-1.83135774191,-0.373566122196588,0.481006384765672));
#9036=CARTESIAN_POINT('Ctrl Pts',(-1.82255520314685,-0.388075792674377,
0.513732289895913));
#9037=CARTESIAN_POINT('Ctrl Pts',(-1.8021878073054,-0.407069005705619,0.581160429138046));
#9038=CARTESIAN_POINT('Ctrl Pts',(-1.79059939410895,-0.411552957311693,
0.615855430396488));
#9039=CARTESIAN_POINT('Ctrl Pts',(-1.76754295572641,-0.411552957311693,
0.679202474225583));
#9040=CARTESIAN_POINT('Ctrl Pts',(-1.75411867833313,-0.407069005705619,
0.713229275562222));
#9041=CARTESIAN_POINT('Ctrl Pts',(-1.72637903628921,-0.388075792674378,
0.777974136626975));
#9042=CARTESIAN_POINT('Ctrl Pts',(-1.71208636586057,-0.373566122196588,
0.808701797248777));
#9043=CARTESIAN_POINT('Ctrl Pts',(-1.68584130567972,-0.339063173951852,
0.862118637580169));
#9044=CARTESIAN_POINT('Ctrl Pts',(-1.67254428069212,-0.317173992396757,
0.88748588628286));
#9045=CARTESIAN_POINT('Ctrl Pts',(-1.64808654453785,-0.266247928944116,
0.932119257848273));
#9046=CARTESIAN_POINT('Ctrl Pts',(-1.63693696192699,-0.237213819614884,
0.951394641067894));
#9047=CARTESIAN_POINT('Ctrl Pts',(-1.61617275903043,-0.166529565724165,
0.986348780151617));
#9048=CARTESIAN_POINT('Ctrl Pts',(-1.60765489827034,-0.123392992551698,
0.999954082314951));
#9049=CARTESIAN_POINT('Ctrl Pts',(-1.60306435598592,-0.07938,1.00725997640701));
#9050=CARTESIAN_POINT('Origin',(-1.80890829501287,-0.07938,0.658388775901912));
#9051=CARTESIAN_POINT('Origin',(0.,-0.07938,0.));
#9052=CARTESIAN_POINT('',(-1.893248,-0.0793799999999999,2.31856010319213E-16));
#9053=CARTESIAN_POINT('Origin',(0.,-0.07938,0.));
#9054=CARTESIAN_POINT('',(-1.8754727744327,-0.07938,-0.258823997855139));
#9055=CARTESIAN_POINT('Origin',(0.,-0.07938,0.));
#9056=CARTESIAN_POINT('Origin',(-1.80890829501287,-0.07938,-0.658388775901913));
#9057=CARTESIAN_POINT('Origin',(-1.80890829501287,0.,-0.658388775901913));
#9058=CARTESIAN_POINT('',(-1.60306435598592,-0.07938,-1.00725997640701));
#9059=CARTESIAN_POINT('Ctrl Pts',(-1.60306435598592,-0.07938,-1.00725997640701));
#9060=CARTESIAN_POINT('Ctrl Pts',(-1.60765489827034,-0.123392992551698,
-0.999954082314952));
#9061=CARTESIAN_POINT('Ctrl Pts',(-1.61617275903043,-0.166529565724166,
-0.986348780151617));
#9062=CARTESIAN_POINT('Ctrl Pts',(-1.63693696192699,-0.237213819614884,
-0.951394641067894));
#9063=CARTESIAN_POINT('Ctrl Pts',(-1.64808654453785,-0.266247928944116,
-0.932119257848273));
#9064=CARTESIAN_POINT('Ctrl Pts',(-1.67254428069212,-0.317173992396757,
-0.88748588628286));
#9065=CARTESIAN_POINT('Ctrl Pts',(-1.68584130567972,-0.339063173951852,
-0.862118637580169));
#9066=CARTESIAN_POINT('Ctrl Pts',(-1.71208636586057,-0.373566122196588,
-0.808701797248777));
#9067=CARTESIAN_POINT('Ctrl Pts',(-1.72637903628921,-0.388075792674377,
-0.777974136626975));
#9068=CARTESIAN_POINT('Ctrl Pts',(-1.75411867833313,-0.407069005705619,
-0.713229275562223));
#9069=CARTESIAN_POINT('Ctrl Pts',(-1.76754295572641,-0.411552957311693,
-0.679202474225584));
#9070=CARTESIAN_POINT('Ctrl Pts',(-1.79059939410895,-0.411552957311693,
-0.615855430396488));
#9071=CARTESIAN_POINT('Ctrl Pts',(-1.8021878073054,-0.407069005705619,-0.581160429138047));
#9072=CARTESIAN_POINT('Ctrl Pts',(-1.82255520314685,-0.388075792674378,
-0.513732289895914));
#9073=CARTESIAN_POINT('Ctrl Pts',(-1.83135774191,-0.373566122196588,-0.481006384765673));
#9074=CARTESIAN_POINT('Ctrl Pts',(-1.84558854251276,-0.339063173951852,
-0.423216711561107));
#9075=CARTESIAN_POINT('Ctrl Pts',(-1.85170818356893,-0.317173992396757,
-0.395237108747477));
#9076=CARTESIAN_POINT('Ctrl Pts',(-1.86166224891746,-0.266247928944116,
-0.34532483272118));
#9077=CARTESIAN_POINT('Ctrl Pts',(-1.86551115062085,-0.237213819614884,
-0.323392218961362));
#9078=CARTESIAN_POINT('Ctrl Pts',(-1.87207293588642,-0.166529565724166,
-0.283268822605344));
#9079=CARTESIAN_POINT('Ctrl Pts',(-1.87429319564052,-0.123392992551698,
-0.267371381128542));
#9080=CARTESIAN_POINT('Ctrl Pts',(-1.8754727744327,-0.07938,-0.258823997855139));
#9081=CARTESIAN_POINT('Origin',(-1.80890829501287,-0.07938,-0.658388775901913));
#9082=CARTESIAN_POINT('Origin',(0.,-0.07938,0.));
#9083=CARTESIAN_POINT('',(-1.27032663816428,-0.07938,-1.40380134701254));
#9084=CARTESIAN_POINT('Origin',(0.,-0.07938,0.));
#9085=CARTESIAN_POINT('Origin',(-0.9625,-0.07938,-1.66709890228504));
#9086=CARTESIAN_POINT('Origin',(-0.9625,0.,-1.66709890228504));
#9087=CARTESIAN_POINT('',(-0.580564309297535,-0.07938,-1.80203581326062));
#9088=CARTESIAN_POINT('Ctrl Pts',(-0.580564309297535,-0.07938,-1.80203581326062));
#9089=CARTESIAN_POINT('Ctrl Pts',(-0.588777006905474,-0.123392992551698,
-1.79938991739155));
#9090=CARTESIAN_POINT('Ctrl Pts',(-0.60404738646464,-0.166529565724165,
-1.79444282663));
#9091=CARTESIAN_POINT('Ctrl Pts',(-0.642421776219619,-0.237213819614884,
-1.78101337496783));
#9092=CARTESIAN_POINT('Ctrl Pts',(-0.663352829527298,-0.266247928944116,
-1.77341438831889));
#9093=CARTESIAN_POINT('Ctrl Pts',(-0.71077832062033,-0.317173992396757,
-1.75494437181449));
#9094=CARTESIAN_POINT('Ctrl Pts',(-0.737270185880015,-0.339063173951852,
-1.74405909481629));
#9095=CARTESIAN_POINT('Ctrl Pts',(-0.791710751504504,-0.373566122196588,
-1.72000942061118));
#9096=CARTESIAN_POINT('Ctrl Pts',(-0.822410931786042,-0.388075792674378,
-1.70565781840267));
#9097=CARTESIAN_POINT('Ctrl Pts',(-0.885277924911194,-0.407069005705619,
-1.67389107556648));
#9098=CARTESIAN_POINT('Ctrl Pts',(-0.917433524307661,-0.411552957311693,
-1.65645399266283));
#9099=CARTESIAN_POINT('Ctrl Pts',(-0.975814475692338,-0.411552957311693,
-1.62274773466534));
#9100=CARTESIAN_POINT('Ctrl Pts',(-1.00699323215303,-0.407069005705619,
-1.60361871016591));
#9101=CARTESIAN_POINT('Ctrl Pts',(-1.06593753500724,-0.388075792674378,
-1.56505766847808));
#9102=CARTESIAN_POINT('Ctrl Pts',(-1.09371647724559,-0.373566122196588,
-1.54564633355776));
#9103=CARTESIAN_POINT('Ctrl Pts',(-1.14176438887219,-0.339063173951852,
-1.51052425783311));
#9104=CARTESIAN_POINT('Ctrl Pts',(-1.1644372479097,-0.317173992396757,-1.49302426802369));
#9105=CARTESIAN_POINT('Ctrl Pts',(-1.20414549695735,-0.266247928944116,
-1.46118759620237));
#9106=CARTESIAN_POINT('Ctrl Pts',(-1.22119193909219,-0.237213819614884,
-1.44686026563443));
#9107=CARTESIAN_POINT('Ctrl Pts',(-1.25200938026802,-0.166529565724166,
-1.42034179508298));
#9108=CARTESIAN_POINT('Ctrl Pts',(-1.26392887632193,-0.123392992551698,
-1.40959080384008));
#9109=CARTESIAN_POINT('Ctrl Pts',(-1.27032663816428,-0.07938,-1.40380134701254));
#9110=CARTESIAN_POINT('Origin',(-0.9625,-0.07938,-1.66709890228504));
#9111=CARTESIAN_POINT('Origin',(0.,-0.07938,0.));
#9112=CARTESIAN_POINT('',(-0.0707805497908242,-0.07938,-1.89192444438865));
#9113=CARTESIAN_POINT('Origin',(0.,-0.07938,0.));
#9114=CARTESIAN_POINT('Origin',(0.334272742008841,-0.07938,-1.8957549245485));
#9115=CARTESIAN_POINT('Origin',(0.334272742008841,0.,-1.8957549245485));
#9116=CARTESIAN_POINT('',(0.71358822996475,-0.07938,-1.75361906569237));
#9117=CARTESIAN_POINT('Ctrl Pts',(0.71358822996475,-0.07938,-1.75361906569237));
#9118=CARTESIAN_POINT('Ctrl Pts',(0.705596189518014,-0.123392992551698,
-1.75687121212928));
#9119=CARTESIAN_POINT('Ctrl Pts',(0.690718471466876,-0.166529565724166,
-1.76289713151763));
#9120=CARTESIAN_POINT('Ctrl Pts',(0.652689698303666,-0.237213819614884,
-1.77727615696148));
#9121=CARTESIAN_POINT('Ctrl Pts',(0.631771046764578,-0.266247928944116,
-1.78490921718958));
#9122=CARTESIAN_POINT('Ctrl Pts',(0.583568715090837,-0.317173992396757,
-1.80124488173997));
#9123=CARTESIAN_POINT('Ctrl Pts',(0.556277847738351,-0.339063173951852,
-1.8099349185301));
#9124=CARTESIAN_POINT('Ctrl Pts',(0.499115122365417,-0.373566122196588,
-1.8265055202942));
#9125=CARTESIAN_POINT('Ctrl Pts',(0.466372387779211,-0.388075792674378,
-1.83524525067263));
#9126=CARTESIAN_POINT('Ctrl Pts',(0.397794208344886,-0.407069005705619,
-1.85132063808607));
#9127=CARTESIAN_POINT('Ctrl Pts',(0.361953249272519,-0.411552957311693,
-1.85863227849762));
#9128=CARTESIAN_POINT('Ctrl Pts',(0.295564880870602,-0.411552957311693,
-1.87033833905209));
#9129=CARTESIAN_POINT('Ctrl Pts',(0.259384667806906,-0.407069005705619,
-1.87572597447038));
#9130=CARTESIAN_POINT('Ctrl Pts',(0.189444152338379,-0.388075792674377,
-1.88407517030084));
#9131=CARTESIAN_POINT('Ctrl Pts',(0.155686882426711,-0.373566122196588,
-1.88706118493262));
#9132=CARTESIAN_POINT('Ctrl Pts',(0.096304011619402,-0.339063173951852,
-1.89104071625784));
#9133=CARTESIAN_POINT('Ctrl Pts',(0.0676868173249583,-0.317173992396757,
-1.89220877917518));
#9134=CARTESIAN_POINT('Ctrl Pts',(0.0168043156156251,-0.266247928944116,
-1.89334444412923));
#9135=CARTESIAN_POINT('Ctrl Pts',(-0.00546344722567807,-0.237213819614884,
-1.89332631395644));
#9136=CARTESIAN_POINT('Ctrl Pts',(-0.0461167210878748,-0.166529565724165,
-1.89282105630055));
#9137=CARTESIAN_POINT('Ctrl Pts',(-0.0621581887675344,-0.123392992551698,
-1.89224702357808));
#9138=CARTESIAN_POINT('Ctrl Pts',(-0.0707805497908242,-0.07938,-1.89192444438865));
#9139=CARTESIAN_POINT('Origin',(0.334272742008841,-0.07938,-1.8957549245485));
#9140=CARTESIAN_POINT('Origin',(0.,-0.07938,0.));
#9141=CARTESIAN_POINT('',(1.16188454446795,-0.07938,-1.49479506783723));
#9142=CARTESIAN_POINT('Origin',(0.,-0.07938,0.));
#9143=CARTESIAN_POINT('Origin',(1.47463555300403,-0.07938,-1.23736614864659));
#9144=CARTESIAN_POINT('Origin',(1.47463555300403,0.,-1.23736614864659));
#9145=CARTESIAN_POINT('',(1.67384490577674,-0.07938,-0.884664467981643));
#9146=CARTESIAN_POINT('Ctrl Pts',(1.67384490577674,-0.07938,-0.884664467981643));
#9147=CARTESIAN_POINT('Ctrl Pts',(1.66981308703787,-0.123392992551698,-0.892292941263125));
#9148=CARTESIAN_POINT('Ctrl Pts',(1.66228948011831,-0.166529565724165,-0.906472276148934));
#9149=CARTESIAN_POINT('Ctrl Pts',(1.64240040915267,-0.237213819614884,-0.941931672888549));
#9150=CARTESIAN_POINT('Ctrl Pts',(1.63128222892223,-0.266247928944116,-0.961225186280958));
#9151=CARTESIAN_POINT('Ctrl Pts',(1.60485746336717,-0.317173992396757,-1.00472289289232));
#9152=CARTESIAN_POINT('Ctrl Pts',(1.58953729406031,-0.339063173951852,-1.02892207867768));
#9153=CARTESIAN_POINT('Ctrl Pts',(1.55639948343386,-0.373566122196588,-1.07835938768384));
#9154=CARTESIAN_POINT('Ctrl Pts',(1.53693488395083,-0.388075792674377,-1.10610103367386));
#9155=CARTESIAN_POINT('Ctrl Pts',(1.49473401052622,-0.407069005705619,-1.16249669890816));
#9156=CARTESIAN_POINT('Ctrl Pts',(1.4719780748558,-0.411552957311693,-1.19113586482651));
#9157=CARTESIAN_POINT('Ctrl Pts',(1.42864614483643,-0.411552957311693,-1.24277684810113));
#9158=CARTESIAN_POINT('Ctrl Pts',(1.40439359896051,-0.407069005705619,-1.27016020894803));
#9159=CARTESIAN_POINT('Ctrl Pts',(1.35618281536764,-0.388075792674378,-1.32151296077672));
#9160=CARTESIAN_POINT('Ctrl Pts',(1.33224261954459,-0.373566122196588,-1.34549913552853));
#9161=CARTESIAN_POINT('Ctrl Pts',(1.28931069477441,-0.339063173951852,-1.38671820696899));
#9162=CARTESIAN_POINT('Ctrl Pts',(1.26813946847809,-0.317173992396757,-1.40600777299249));
#9163=CARTESIAN_POINT('Ctrl Pts',(1.22989120215289,-0.266247928944116,-1.4395843844684));
#9164=CARTESIAN_POINT('Ctrl Pts',(1.21282145231718,-0.237213819614884,-1.45388393800011));
#9165=CARTESIAN_POINT('Ctrl Pts',(1.18135446441955,-0.166529565724166,-1.47962830891229));
#9166=CARTESIAN_POINT('Ctrl Pts',(1.16869700612251,-0.123392992551698,-1.48949983100074));
#9167=CARTESIAN_POINT('Ctrl Pts',(1.16188454446795,-0.0793799999999999,
-1.49479506783723));
#9168=CARTESIAN_POINT('Origin',(1.47463555300403,-0.07938,-1.23736614864659));
#9169=CARTESIAN_POINT('Origin',(0.,-0.27783,0.));
#9170=CARTESIAN_POINT('',(-1.893248,-0.47628,2.31856010319213E-16));
#9171=CARTESIAN_POINT('Origin',(0.,-0.47628,0.));
#9172=CARTESIAN_POINT('',(-1.893248,-0.27783,2.31856010319213E-16));
#9173=CARTESIAN_POINT('',(1.85089094746182,-0.07938,0.39823446624808));
#9174=CARTESIAN_POINT('Origin',(0.,-0.07938,0.));
#9175=CARTESIAN_POINT('',(1.85089094746182,-0.07938,-0.39823446624808));
#9176=CARTESIAN_POINT('Ctrl Pts',(1.85089094746182,-0.07938,0.39823446624808));
#9177=CARTESIAN_POINT('Ctrl Pts',(1.8527058832274,-0.123392992551698,0.38979911355147));
#9178=CARTESIAN_POINT('Ctrl Pts',(1.85605676673266,-0.166529565724166,0.374101031547026));
#9179=CARTESIAN_POINT('Ctrl Pts',(1.86361371531181,-0.237213819614884,0.334153109333404));
#9180=CARTESIAN_POINT('Ctrl Pts',(1.86749832648465,-0.266247928944116,0.312226792116516));
#9181=CARTESIAN_POINT('Ctrl Pts',(1.87521556853004,-0.317173992396757,0.261920103790797));
#9182=CARTESIAN_POINT('Ctrl Pts',(1.87903457475221,-0.339063173951852,0.233534836983177));
#9183=CARTESIAN_POINT('Ctrl Pts',(1.88542722875009,-0.373566122196588,0.174363087053423));
#9184=CARTESIAN_POINT('Ctrl Pts',(1.88834846679328,-0.388075792674378,0.140600149924591));
#9185=CARTESIAN_POINT('Ctrl Pts',(1.89227115706422,-0.407069005705619,0.0702723654005715));
#9186=CARTESIAN_POINT('Ctrl Pts',(1.893248,-0.411552957311693,0.0337062579974903));
#9187=CARTESIAN_POINT('Ctrl Pts',(1.893248,-0.411552957311693,-0.0337062579974903));
#9188=CARTESIAN_POINT('Ctrl Pts',(1.89227115706422,-0.407069005705619,-0.0702723654005715));
#9189=CARTESIAN_POINT('Ctrl Pts',(1.88834846679328,-0.388075792674378,-0.140600149924591));
#9190=CARTESIAN_POINT('Ctrl Pts',(1.88542722875009,-0.373566122196588,-0.174363087053422));
#9191=CARTESIAN_POINT('Ctrl Pts',(1.87903457475221,-0.339063173951852,-0.233534836983177));
#9192=CARTESIAN_POINT('Ctrl Pts',(1.87521556853004,-0.317173992396757,-0.261920103790797));
#9193=CARTESIAN_POINT('Ctrl Pts',(1.86749832648465,-0.266247928944116,-0.312226792116516));
#9194=CARTESIAN_POINT('Ctrl Pts',(1.86361371531181,-0.237213819614884,-0.334153109333404));
#9195=CARTESIAN_POINT('Ctrl Pts',(1.85605676673266,-0.166529565724166,-0.374101031547026));
#9196=CARTESIAN_POINT('Ctrl Pts',(1.8527058832274,-0.123392992551698,-0.38979911355147));
#9197=CARTESIAN_POINT('Ctrl Pts',(1.85089094746182,-0.07938,-0.39823446624808));
#9198=CARTESIAN_POINT('Origin',(0.,-0.07938,0.));
#9199=CARTESIAN_POINT('Origin',(0.,-0.07938,0.));
#9200=CARTESIAN_POINT('Origin',(1.925,-0.07938,0.));
#9201=CARTESIAN_POINT('Origin',(1.925,0.,0.));
#9202=CARTESIAN_POINT('Origin',(1.925,-0.07938,0.));
#9203=CARTESIAN_POINT('Origin',(0.,-0.47628,0.));
#9204=CARTESIAN_POINT('Origin',(0.,-0.07938,0.));
#9205=CARTESIAN_POINT('',(0.,0.,0.));
#9206=CARTESIAN_POINT('Origin',(1.95469,0.745,0.));
#9207=CARTESIAN_POINT('',(-1.95469,0.745,-2.39380485182534E-16));
#9208=CARTESIAN_POINT('Origin',(0.,0.745,0.));
#9209=CARTESIAN_POINT('',(-1.90031,0.745,-2.32720855888771E-16));
#9210=CARTESIAN_POINT('Origin',(0.,0.745,0.));
#9211=CARTESIAN_POINT('Origin',(0.,0.7075,0.));
#9212=CARTESIAN_POINT('',(-1.95469,0.67,-2.39380485182534E-16));
#9213=CARTESIAN_POINT('Origin',(0.,0.67,0.));
#9214=CARTESIAN_POINT('',(-1.95469,0.7075,-2.39380485182534E-16));
#9215=CARTESIAN_POINT('Origin',(1.90031,0.67,0.));
#9216=CARTESIAN_POINT('',(-1.90031,0.67,-2.32720855888771E-16));
#9217=CARTESIAN_POINT('Origin',(0.,0.67,0.));
#9218=CARTESIAN_POINT('Origin',(0.,0.7075,0.));
#9219=CARTESIAN_POINT('',(-1.90031,0.7075,-2.32720855888771E-16));
#9220=CARTESIAN_POINT('Origin',(1.95469,-0.67,0.));
#9221=CARTESIAN_POINT('',(-1.95469,-0.67,-2.39380485182534E-16));
#9222=CARTESIAN_POINT('Origin',(0.,-0.67,0.));
#9223=CARTESIAN_POINT('',(-1.90031,-0.67,-2.32720855888771E-16));
#9224=CARTESIAN_POINT('Origin',(0.,-0.67,0.));
#9225=CARTESIAN_POINT('Origin',(0.,-0.7075,0.));
#9226=CARTESIAN_POINT('',(-1.95469,-0.745,-2.39380485182534E-16));
#9227=CARTESIAN_POINT('Origin',(0.,-0.745,0.));
#9228=CARTESIAN_POINT('',(-1.95469,-0.7075,-2.39380485182534E-16));
#9229=CARTESIAN_POINT('Origin',(1.90031,-0.745,0.));
#9230=CARTESIAN_POINT('',(-1.90031,-0.745,-2.32720855888771E-16));
#9231=CARTESIAN_POINT('Origin',(0.,-0.745,0.));
#9232=CARTESIAN_POINT('Origin',(0.,-0.7075,0.));
#9233=CARTESIAN_POINT('',(-1.90031,-0.7075,-2.32720855888771E-16));
#9234=CARTESIAN_POINT('',(0.,0.,0.));
#9235=CARTESIAN_POINT('',(0.,0.,0.));
#9236=CARTESIAN_POINT('',(0.,0.,0.));
#9237=CARTESIAN_POINT('',(0.,0.,0.));
#9238=CARTESIAN_POINT('',(0.,0.,0.));
#9239=CARTESIAN_POINT('',(0.,0.,0.));
#9240=CARTESIAN_POINT('Origin',(0.,-0.5,0.));
#9241=CARTESIAN_POINT('',(-0.24505,-0.5,3.00099698131059E-17));
#9242=CARTESIAN_POINT('Origin',(0.,-0.5,0.));
#9243=CARTESIAN_POINT('Origin',(0.0721687836487032,0.,-0.125));
#9244=CARTESIAN_POINT('',(0.0721687836487032,0.,-0.125));
#9245=CARTESIAN_POINT('',(0.144337567297406,0.,0.));
#9246=CARTESIAN_POINT('',(0.117710979560879,0.,-0.0461186027918559));
#9247=CARTESIAN_POINT('',(0.0721687836487032,-0.25,-0.125));
#9248=CARTESIAN_POINT('',(0.0721687836487032,0.,-0.125));
#9249=CARTESIAN_POINT('',(0.144337567297406,-0.25,0.));
#9250=CARTESIAN_POINT('',(0.144337567297406,-0.25,0.));
#9251=CARTESIAN_POINT('',(0.144337567297406,0.,0.));
#9252=CARTESIAN_POINT('Origin',(-0.0721687836487032,0.,-0.125));
#9253=CARTESIAN_POINT('',(-0.0721687836487032,0.,-0.125));
#9254=CARTESIAN_POINT('',(0.0739156081756484,0.,-0.125));
#9255=CARTESIAN_POINT('',(-0.0721687836487032,-0.25,-0.125));
#9256=CARTESIAN_POINT('',(-0.0721687836487032,0.,-0.125));
#9257=CARTESIAN_POINT('',(0.0721687836487032,-0.25,-0.125));
#9258=CARTESIAN_POINT('Origin',(-0.144337567297406,0.,-4.16333634234434E-17));
#9259=CARTESIAN_POINT('',(-0.144337567297406,0.,-1.76762539787485E-17));
#9260=CARTESIAN_POINT('',(-0.0987953713852306,0.,-0.0788813972081442));
#9261=CARTESIAN_POINT('',(-0.144337567297406,-0.25,-2.77555756156289E-17));
#9262=CARTESIAN_POINT('',(-0.144337567297406,0.,-1.76762539787485E-17));
#9263=CARTESIAN_POINT('',(-0.0721687836487032,-0.25,-0.125));
#9264=CARTESIAN_POINT('Origin',(-0.0721687836487033,0.,0.125));
#9265=CARTESIAN_POINT('',(-0.0721687836487033,0.,0.125));
#9266=CARTESIAN_POINT('',(-0.0627109795608791,0.,0.141381397208144));
#9267=CARTESIAN_POINT('',(-0.0721687836487033,-0.25,0.125));
#9268=CARTESIAN_POINT('',(-0.0721687836487033,0.,0.125));
#9269=CARTESIAN_POINT('',(-0.144337567297406,-0.25,-1.76762539787485E-17));
#9270=CARTESIAN_POINT('Origin',(0.0721687836487032,0.,0.125));
#9271=CARTESIAN_POINT('',(0.0721687836487032,0.,0.125));
#9272=CARTESIAN_POINT('',(0.146084391824352,0.,0.125));
#9273=CARTESIAN_POINT('',(0.0721687836487032,-0.25,0.125));
#9274=CARTESIAN_POINT('',(0.0721687836487032,0.,0.125));
#9275=CARTESIAN_POINT('',(-0.0721687836487033,-0.25,0.125));
#9276=CARTESIAN_POINT('Origin',(0.144337567297406,0.,0.));
#9277=CARTESIAN_POINT('',(0.153795371385231,0.,-0.0163813972081441));
#9278=CARTESIAN_POINT('',(0.0721687836487032,-0.25,0.125));
#9279=CARTESIAN_POINT('Origin',(0.,-0.25,0.));
#9280=CARTESIAN_POINT('Origin',(0.22,0.,0.));
#9281=CARTESIAN_POINT('',(-0.22,-8.67361737988404E-18,-2.69422295812418E-17));
#9282=CARTESIAN_POINT('Origin',(0.,0.,0.));
#9283=CARTESIAN_POINT('Origin',(0.,-0.015,0.));
#9284=CARTESIAN_POINT('',(-0.24505,-0.02505,-3.00099698131059E-17));
#9285=CARTESIAN_POINT('Origin',(0.,-0.02505,0.));
#9286=CARTESIAN_POINT('',(-0.235,-0.015,-2.87791997799628E-17));
#9287=CARTESIAN_POINT('Origin',(0.,-0.3775,0.));
#9288=CARTESIAN_POINT('',(-0.24505,-0.3775,-3.00099698131059E-17));
#9289=CARTESIAN_POINT('',(0.,0.,0.));
#9290=CARTESIAN_POINT('',(0.,0.,0.));
#9291=CARTESIAN_POINT('Origin',(-6.95466594928129,-1.86349712473815,6.4));
#9292=CARTESIAN_POINT('',(-7.11966594928129,-1.86349712473815,6.5));
#9293=CARTESIAN_POINT('Origin',(-6.95466594928129,-1.86349712473815,6.5));
#9294=CARTESIAN_POINT('',(-7.11966594928129,-1.86349712473815,7.6));
#9295=CARTESIAN_POINT('',(-7.11966594928129,-1.86349712473815,6.4));
#9296=CARTESIAN_POINT('Origin',(-6.95466594928129,-1.86349712473815,7.6));
#9297=CARTESIAN_POINT('Origin',(-6.95466594928129,-1.86349712473815,7.6));
#9298=CARTESIAN_POINT('Origin',(-1.86349712473815,6.95466594928129,6.4));
#9299=CARTESIAN_POINT('',(-2.02849712473815,6.95466594928129,6.5));
#9300=CARTESIAN_POINT('Origin',(-1.86349712473815,6.95466594928129,6.5));
#9301=CARTESIAN_POINT('',(-2.02849712473815,6.95466594928129,7.6));
#9302=CARTESIAN_POINT('',(-2.02849712473815,6.95466594928129,6.4));
#9303=CARTESIAN_POINT('Origin',(-1.86349712473815,6.95466594928129,7.6));
#9304=CARTESIAN_POINT('Origin',(-1.86349712473815,6.95466594928129,7.6));
#9305=CARTESIAN_POINT('Origin',(6.95466594928129,1.86349712473815,6.4));
#9306=CARTESIAN_POINT('',(6.78966594928129,1.86349712473815,6.5));
#9307=CARTESIAN_POINT('Origin',(6.95466594928129,1.86349712473815,6.5));
#9308=CARTESIAN_POINT('',(6.78966594928129,1.86349712473815,7.6));
#9309=CARTESIAN_POINT('',(6.78966594928129,1.86349712473815,6.4));
#9310=CARTESIAN_POINT('Origin',(6.95466594928129,1.86349712473815,7.6));
#9311=CARTESIAN_POINT('Origin',(6.95466594928129,1.86349712473815,7.6));
#9312=CARTESIAN_POINT('Origin',(1.86349712473815,-6.95466594928129,6.4));
#9313=CARTESIAN_POINT('',(1.69849712473815,-6.95466594928129,6.5));
#9314=CARTESIAN_POINT('Origin',(1.86349712473815,-6.95466594928129,6.5));
#9315=CARTESIAN_POINT('',(1.69849712473815,-6.95466594928129,7.6));
#9316=CARTESIAN_POINT('',(1.69849712473815,-6.95466594928129,6.4));
#9317=CARTESIAN_POINT('Origin',(1.86349712473815,-6.95466594928129,7.6));
#9318=CARTESIAN_POINT('Origin',(1.86349712473815,-6.95466594928129,7.6));
#9319=CARTESIAN_POINT('Origin',(3.6,-6.23538290724796,6.4));
#9320=CARTESIAN_POINT('',(3.29,-6.23538290724796,6.5));
#9321=CARTESIAN_POINT('Origin',(3.6,-6.23538290724796,6.5));
#9322=CARTESIAN_POINT('',(3.29,-6.23538290724796,7.2));
#9323=CARTESIAN_POINT('',(3.29,-6.23538290724796,6.4));
#9324=CARTESIAN_POINT('Origin',(3.6,-6.23538290724796,7.2));
#9325=CARTESIAN_POINT('Origin',(3.6,-6.23538290724796,7.2));
#9326=CARTESIAN_POINT('Origin',(-3.6,-6.23538290724796,6.4));
#9327=CARTESIAN_POINT('',(-3.91,-6.23538290724796,6.5));
#9328=CARTESIAN_POINT('Origin',(-3.6,-6.23538290724796,6.5));
#9329=CARTESIAN_POINT('',(-3.91,-6.23538290724796,7.2));
#9330=CARTESIAN_POINT('',(-3.91,-6.23538290724796,6.4));
#9331=CARTESIAN_POINT('Origin',(-3.6,-6.23538290724796,7.2));
#9332=CARTESIAN_POINT('Origin',(-3.6,-6.23538290724796,7.2));
#9333=CARTESIAN_POINT('Origin',(-7.2,8.81745695386094E-16,6.4));
#9334=CARTESIAN_POINT('',(-7.51,8.43781644612526E-16,6.5));
#9335=CARTESIAN_POINT('Origin',(-7.2,8.81745695386094E-16,6.5));
#9336=CARTESIAN_POINT('',(-7.51,8.43781644612526E-16,7.2));
#9337=CARTESIAN_POINT('',(-7.51,8.43781644612526E-16,6.4));
#9338=CARTESIAN_POINT('Origin',(-7.2,8.81745695386094E-16,7.2));
#9339=CARTESIAN_POINT('Origin',(-7.2,8.88178419700125E-16,7.2));
#9340=CARTESIAN_POINT('Origin',(-6.23538290724796,3.6,6.4));
#9341=CARTESIAN_POINT('',(-6.54538290724796,3.6,6.5));
#9342=CARTESIAN_POINT('Origin',(-6.23538290724796,3.6,6.5));
#9343=CARTESIAN_POINT('',(-6.54538290724796,3.6,7.2));
#9344=CARTESIAN_POINT('',(-6.54538290724796,3.6,6.4));
#9345=CARTESIAN_POINT('Origin',(-6.23538290724796,3.6,7.2));
#9346=CARTESIAN_POINT('Origin',(-6.23538290724796,3.6,7.2));
#9347=CARTESIAN_POINT('Origin',(4.40872847693047E-16,7.2,6.4));
#9348=CARTESIAN_POINT('',(-0.31,7.2,6.5));
#9349=CARTESIAN_POINT('Origin',(4.40872847693047E-16,7.2,6.5));
#9350=CARTESIAN_POINT('',(-0.31,7.2,7.2));
#9351=CARTESIAN_POINT('',(-0.31,7.2,6.4));
#9352=CARTESIAN_POINT('Origin',(4.40872847693047E-16,7.2,7.2));
#9353=CARTESIAN_POINT('Origin',(4.44089209850063E-16,7.2,7.2));
#9354=CARTESIAN_POINT('Origin',(6.23538290724796,3.6,6.4));
#9355=CARTESIAN_POINT('',(5.92538290724796,3.6,6.5));
#9356=CARTESIAN_POINT('Origin',(6.23538290724796,3.6,6.5));
#9357=CARTESIAN_POINT('',(5.92538290724796,3.6,7.2));
#9358=CARTESIAN_POINT('',(5.92538290724796,3.6,6.4));
#9359=CARTESIAN_POINT('Origin',(6.23538290724796,3.6,7.2));
#9360=CARTESIAN_POINT('Origin',(6.23538290724796,3.6,7.2));
#9361=CARTESIAN_POINT('Origin',(3.6,6.23538290724796,6.4));
#9362=CARTESIAN_POINT('',(3.29,6.23538290724796,6.5));
#9363=CARTESIAN_POINT('Origin',(3.6,6.23538290724796,6.5));
#9364=CARTESIAN_POINT('',(3.29,6.23538290724796,7.2));
#9365=CARTESIAN_POINT('',(3.29,6.23538290724796,6.4));
#9366=CARTESIAN_POINT('Origin',(3.6,6.23538290724796,7.2));
#9367=CARTESIAN_POINT('Origin',(3.6,6.23538290724796,7.2));
#9368=CARTESIAN_POINT('Origin',(-3.6,6.23538290724796,6.4));
#9369=CARTESIAN_POINT('',(-3.91,6.23538290724796,6.5));
#9370=CARTESIAN_POINT('Origin',(-3.6,6.23538290724796,6.5));
#9371=CARTESIAN_POINT('',(-3.91,6.23538290724796,7.2));
#9372=CARTESIAN_POINT('',(-3.91,6.23538290724796,6.4));
#9373=CARTESIAN_POINT('Origin',(-3.6,6.23538290724796,7.2));
#9374=CARTESIAN_POINT('Origin',(-3.6,6.23538290724796,7.2));
#9375=CARTESIAN_POINT('Origin',(7.2,0.,6.4));
#9376=CARTESIAN_POINT('',(6.89,-3.79640507735679E-17,6.5));
#9377=CARTESIAN_POINT('Origin',(7.2,0.,6.5));
#9378=CARTESIAN_POINT('',(6.89,-3.79640507735679E-17,7.2));
#9379=CARTESIAN_POINT('',(6.89,-3.79640507735679E-17,6.4));
#9380=CARTESIAN_POINT('Origin',(7.2,0.,7.2));
#9381=CARTESIAN_POINT('Origin',(7.2,0.,7.2));
#9382=CARTESIAN_POINT('Origin',(-6.23538290724796,-3.6,6.4));
#9383=CARTESIAN_POINT('',(-6.54538290724796,-3.6,6.5));
#9384=CARTESIAN_POINT('Origin',(-6.23538290724796,-3.6,6.5));
#9385=CARTESIAN_POINT('',(-6.54538290724796,-3.6,7.2));
#9386=CARTESIAN_POINT('',(-6.54538290724796,-3.6,6.4));
#9387=CARTESIAN_POINT('Origin',(-6.23538290724796,-3.6,7.2));
#9388=CARTESIAN_POINT('Origin',(-6.23538290724796,-3.6,7.2));
#9389=CARTESIAN_POINT('Origin',(-1.32261854307914E-15,-7.2,6.4));
#9390=CARTESIAN_POINT('',(-0.310000000000001,-7.2,6.5));
#9391=CARTESIAN_POINT('Origin',(-1.32261854307914E-15,-7.2,6.5));
#9392=CARTESIAN_POINT('',(-0.310000000000001,-7.2,7.2));
#9393=CARTESIAN_POINT('',(-0.310000000000001,-7.2,6.4));
#9394=CARTESIAN_POINT('Origin',(-1.32261854307914E-15,-7.2,7.2));
#9395=CARTESIAN_POINT('Origin',(-1.33226762955019E-15,-7.2,7.2));
#9396=CARTESIAN_POINT('Origin',(6.23538290724796,-3.6,6.4));
#9397=CARTESIAN_POINT('',(5.92538290724796,-3.6,6.5));
#9398=CARTESIAN_POINT('Origin',(6.23538290724796,-3.6,6.5));
#9399=CARTESIAN_POINT('',(5.92538290724796,-3.6,7.2));
#9400=CARTESIAN_POINT('',(5.92538290724796,-3.6,6.4));
#9401=CARTESIAN_POINT('Origin',(6.23538290724796,-3.6,7.2));
#9402=CARTESIAN_POINT('Origin',(6.23538290724796,-3.6,7.2));
#9403=CARTESIAN_POINT('Origin',(-2.33345237791561,-2.33345237791561,2.9));
#9404=CARTESIAN_POINT('',(-2.49845237791561,-2.33345237791561,3.));
#9405=CARTESIAN_POINT('Origin',(-2.33345237791561,-2.33345237791561,3.));
#9406=CARTESIAN_POINT('',(-2.49845237791561,-2.33345237791561,4.7));
#9407=CARTESIAN_POINT('',(-2.49845237791561,-2.33345237791561,2.9));
#9408=CARTESIAN_POINT('Origin',(-2.33345237791561,-2.33345237791561,4.7));
#9409=CARTESIAN_POINT('Origin',(-2.33345237791561,-2.33345237791561,4.7));
#9410=CARTESIAN_POINT('Origin',(-2.33345237791561,2.33345237791561,2.9));
#9411=CARTESIAN_POINT('',(-2.49845237791561,2.33345237791561,3.));
#9412=CARTESIAN_POINT('Origin',(-2.33345237791561,2.33345237791561,3.));
#9413=CARTESIAN_POINT('',(-2.49845237791561,2.33345237791561,4.7));
#9414=CARTESIAN_POINT('',(-2.49845237791561,2.33345237791561,2.9));
#9415=CARTESIAN_POINT('Origin',(-2.33345237791561,2.33345237791561,4.7));
#9416=CARTESIAN_POINT('Origin',(-2.33345237791561,2.33345237791561,4.7));
#9417=CARTESIAN_POINT('Origin',(2.33345237791561,2.33345237791561,2.9));
#9418=CARTESIAN_POINT('',(2.16845237791561,2.33345237791561,3.));
#9419=CARTESIAN_POINT('Origin',(2.33345237791561,2.33345237791561,3.));
#9420=CARTESIAN_POINT('',(2.16845237791561,2.33345237791561,4.7));
#9421=CARTESIAN_POINT('',(2.16845237791561,2.33345237791561,2.9));
#9422=CARTESIAN_POINT('Origin',(2.33345237791561,2.33345237791561,4.7));
#9423=CARTESIAN_POINT('Origin',(2.33345237791561,2.33345237791561,4.7));
#9424=CARTESIAN_POINT('Origin',(2.33345237791561,-2.33345237791561,2.9));
#9425=CARTESIAN_POINT('',(2.16845237791561,-2.33345237791561,3.));
#9426=CARTESIAN_POINT('Origin',(2.33345237791561,-2.33345237791561,3.));
#9427=CARTESIAN_POINT('',(2.16845237791561,-2.33345237791561,4.7));
#9428=CARTESIAN_POINT('',(2.16845237791561,-2.33345237791561,2.9));
#9429=CARTESIAN_POINT('Origin',(2.33345237791561,-2.33345237791561,4.7));
#9430=CARTESIAN_POINT('Origin',(2.33345237791561,-2.33345237791561,4.7));
#9431=CARTESIAN_POINT('Origin',(-1.56142466891288E-15,-8.5,6.4));
#9432=CARTESIAN_POINT('',(-0.330000000000002,-8.5,6.5));
#9433=CARTESIAN_POINT('Origin',(-1.56142466891288E-15,-8.5,6.5));
#9434=CARTESIAN_POINT('',(-0.330000000000002,-8.5,7.7));
#9435=CARTESIAN_POINT('',(-0.330000000000002,-8.5,6.4));
#9436=CARTESIAN_POINT('Origin',(-1.56142466891288E-15,-8.5,7.7));
#9437=CARTESIAN_POINT('Origin',(-8.5,1.04094977927525E-15,6.4));
#9438=CARTESIAN_POINT('',(-8.83,1.00053643490339E-15,6.5));
#9439=CARTESIAN_POINT('Origin',(-8.5,1.04094977927525E-15,6.5));
#9440=CARTESIAN_POINT('',(-8.83,1.08136312364711E-15,7.7));
#9441=CARTESIAN_POINT('',(-8.83,1.00053643490339E-15,6.4));
#9442=CARTESIAN_POINT('Origin',(-8.5,1.04094977927525E-15,7.7));
#9443=CARTESIAN_POINT('Origin',(-6.01040764008565,6.01040764008565,6.4));
#9444=CARTESIAN_POINT('',(-6.34040764008565,6.01040764008565,6.5));
#9445=CARTESIAN_POINT('Origin',(-6.01040764008565,6.01040764008565,6.5));
#9446=CARTESIAN_POINT('',(-6.34040764008565,6.01040764008565,7.7));
#9447=CARTESIAN_POINT('',(-6.34040764008565,6.01040764008565,6.4));
#9448=CARTESIAN_POINT('Origin',(-6.01040764008565,6.01040764008565,7.7));
#9449=CARTESIAN_POINT('Origin',(6.01040764008565,6.01040764008565,6.4));
#9450=CARTESIAN_POINT('',(5.68040764008565,6.01040764008565,6.5));
#9451=CARTESIAN_POINT('Origin',(6.01040764008565,6.01040764008565,6.5));
#9452=CARTESIAN_POINT('',(5.68040764008565,6.01040764008565,7.7));
#9453=CARTESIAN_POINT('',(5.68040764008565,6.01040764008565,6.4));
#9454=CARTESIAN_POINT('Origin',(6.01040764008565,6.01040764008565,7.7));
#9455=CARTESIAN_POINT('Origin',(5.20474889637625E-16,8.5,6.4));
#9456=CARTESIAN_POINT('',(-0.329999999999999,8.5,6.5));
#9457=CARTESIAN_POINT('Origin',(5.20474889637625E-16,8.5,6.5));
#9458=CARTESIAN_POINT('',(-0.329999999999999,8.5,7.7));
#9459=CARTESIAN_POINT('',(-0.329999999999999,8.5,6.4));
#9460=CARTESIAN_POINT('Origin',(5.20474889637625E-16,8.5,7.7));
#9461=CARTESIAN_POINT('Origin',(8.5,0.,6.4));
#9462=CARTESIAN_POINT('',(8.17,-4.04133443718627E-17,6.5));
#9463=CARTESIAN_POINT('Origin',(8.5,0.,6.5));
#9464=CARTESIAN_POINT('',(8.17,4.04133443718627E-17,7.7));
#9465=CARTESIAN_POINT('',(8.17,-4.04133443718627E-17,6.4));
#9466=CARTESIAN_POINT('Origin',(8.5,0.,7.7));
#9467=CARTESIAN_POINT('Origin',(-6.01040764008566,-6.01040764008565,6.4));
#9468=CARTESIAN_POINT('',(-6.34040764008566,-6.01040764008565,6.5));
#9469=CARTESIAN_POINT('Origin',(-6.01040764008566,-6.01040764008565,6.5));
#9470=CARTESIAN_POINT('',(-6.34040764008566,-6.01040764008565,7.7));
#9471=CARTESIAN_POINT('',(-6.34040764008566,-6.01040764008565,6.4));
#9472=CARTESIAN_POINT('Origin',(-6.01040764008566,-6.01040764008565,7.7));
#9473=CARTESIAN_POINT('Origin',(6.01040764008565,-6.01040764008566,6.4));
#9474=CARTESIAN_POINT('',(5.68040764008565,-6.01040764008566,6.5));
#9475=CARTESIAN_POINT('Origin',(6.01040764008565,-6.01040764008566,6.5));
#9476=CARTESIAN_POINT('',(5.68040764008565,-6.01040764008566,7.7));
#9477=CARTESIAN_POINT('',(5.68040764008565,-6.01040764008566,6.4));
#9478=CARTESIAN_POINT('Origin',(6.01040764008565,-6.01040764008566,7.7));
#9479=CARTESIAN_POINT('Origin',(0.,0.,6.5));
#9480=CARTESIAN_POINT('',(-2.,-2.44929359829471E-16,6.5));
#9481=CARTESIAN_POINT('Origin',(0.,0.,6.5));
#9482=CARTESIAN_POINT('',(-1.9,-2.32682891837997E-16,6.5));
#9483=CARTESIAN_POINT('Origin',(0.,0.,6.5));
#9484=CARTESIAN_POINT('Origin',(0.,0.,6.25));
#9485=CARTESIAN_POINT('',(-1.9,-2.32682891837997E-16,6.25));
#9486=CARTESIAN_POINT('',(-1.9,-2.32682891837997E-16,6.25));
#9487=CARTESIAN_POINT('Origin',(0.,0.,6.25));
#9488=CARTESIAN_POINT('Origin',(0.,0.,6.25));
#9489=CARTESIAN_POINT('',(-2.6,-3.18408167778312E-16,6.25));
#9490=CARTESIAN_POINT('Origin',(0.,0.,6.25));
#9491=CARTESIAN_POINT('Origin',(0.,0.,6.5));
#9492=CARTESIAN_POINT('',(-10.,-1.22464679914735E-15,6.5));
#9493=CARTESIAN_POINT('Origin',(0.,0.,6.5));
#9494=CARTESIAN_POINT('',(-4.,-4.89858719658941E-16,6.5));
#9495=CARTESIAN_POINT('Origin',(0.,0.,6.5));
#9496=CARTESIAN_POINT('Origin',(0.,0.,6.5));
#9497=CARTESIAN_POINT('',(-2.,-2.44929359829471E-16,7.7));
#9498=CARTESIAN_POINT('Origin',(0.,0.,7.7));
#9499=CARTESIAN_POINT('',(-2.,-2.44929359829471E-16,6.5));
#9500=CARTESIAN_POINT('Origin',(0.,0.,6.5));
#9501=CARTESIAN_POINT('',(-10.,-1.22464679914735E-15,7.7));
#9502=CARTESIAN_POINT('Origin',(0.,0.,7.7));
#9503=CARTESIAN_POINT('',(-10.,-1.22464679914735E-15,6.5));
#9504=CARTESIAN_POINT('Origin',(0.,0.,7.7));
#9505=CARTESIAN_POINT('Origin',(0.,0.,3.));
#9506=CARTESIAN_POINT('',(-2.6,-3.18408167778312E-16,3.));
#9507=CARTESIAN_POINT('',(-2.6,-3.18408167778312E-16,3.));
#9508=CARTESIAN_POINT('Origin',(0.,0.,3.));
#9509=CARTESIAN_POINT('Origin',(0.,0.,3.));
#9510=CARTESIAN_POINT('',(-4.,-4.89858719658941E-16,3.));
#9511=CARTESIAN_POINT('',(-4.,-4.89858719658941E-16,3.));
#9512=CARTESIAN_POINT('Origin',(0.,0.,3.));
#9513=CARTESIAN_POINT('Origin',(0.,0.,3.));
#9514=CARTESIAN_POINT('',(0.,0.,0.));
#9515=CARTESIAN_POINT('Origin',(0.,0.,4.75));
#9516=CARTESIAN_POINT('',(-2.,-2.44929359829471E-16,6.25));
#9517=CARTESIAN_POINT('Origin',(0.,0.,6.25));
#9518=CARTESIAN_POINT('',(-2.,-2.44929359829471E-16,4.75));
#9519=CARTESIAN_POINT('',(-2.,-2.44929359829471E-16,4.75));
#9520=CARTESIAN_POINT('Origin',(0.,0.,4.75));
#9521=CARTESIAN_POINT('Origin',(0.,0.,4.75));
#9522=CARTESIAN_POINT('',(-2.59,-3.17183520979164E-16,6.25));
#9523=CARTESIAN_POINT('Origin',(0.,0.,6.25));
#9524=CARTESIAN_POINT('',(-2.59,-3.17183520979164E-16,4.75));
#9525=CARTESIAN_POINT('',(-2.59,-3.17183520979164E-16,4.75));
#9526=CARTESIAN_POINT('Origin',(0.,0.,4.75));
#9527=CARTESIAN_POINT('Origin',(0.,0.,6.25));
#9528=CARTESIAN_POINT('Origin',(0.,0.,4.75));
#9529=CARTESIAN_POINT('',(0.,0.,0.));
#9530=CARTESIAN_POINT('Origin',(-2.33345237791561,-2.33345237791561,2.6));
#9531=CARTESIAN_POINT('',(-2.55845237791561,-2.33345237791561,2.7));
#9532=CARTESIAN_POINT('Origin',(-2.33345237791561,-2.33345237791561,2.7));
#9533=CARTESIAN_POINT('',(-2.55845237791561,-2.33345237791561,3.));
#9534=CARTESIAN_POINT('',(-2.55845237791561,-2.33345237791561,2.6));
#9535=CARTESIAN_POINT('Origin',(-2.33345237791561,-2.33345237791561,3.));
#9536=CARTESIAN_POINT('Origin',(-2.33345237791561,2.33345237791561,2.6));
#9537=CARTESIAN_POINT('',(-2.55845237791561,2.33345237791561,2.7));
#9538=CARTESIAN_POINT('Origin',(-2.33345237791561,2.33345237791561,2.7));
#9539=CARTESIAN_POINT('',(-2.55845237791561,2.33345237791561,3.));
#9540=CARTESIAN_POINT('',(-2.55845237791561,2.33345237791561,2.6));
#9541=CARTESIAN_POINT('Origin',(-2.33345237791561,2.33345237791561,3.));
#9542=CARTESIAN_POINT('Origin',(2.33345237791561,2.33345237791561,2.6));
#9543=CARTESIAN_POINT('',(2.10845237791561,2.33345237791561,2.7));
#9544=CARTESIAN_POINT('Origin',(2.33345237791561,2.33345237791561,2.7));
#9545=CARTESIAN_POINT('',(2.10845237791561,2.33345237791561,3.));
#9546=CARTESIAN_POINT('',(2.10845237791561,2.33345237791561,2.6));
#9547=CARTESIAN_POINT('Origin',(2.33345237791561,2.33345237791561,3.));
#9548=CARTESIAN_POINT('Origin',(2.33345237791561,-2.33345237791561,2.6));
#9549=CARTESIAN_POINT('',(2.10845237791561,-2.33345237791561,2.7));
#9550=CARTESIAN_POINT('Origin',(2.33345237791561,-2.33345237791561,2.7));
#9551=CARTESIAN_POINT('',(2.10845237791561,-2.33345237791561,3.));
#9552=CARTESIAN_POINT('',(2.10845237791561,-2.33345237791561,2.6));
#9553=CARTESIAN_POINT('Origin',(2.33345237791561,-2.33345237791561,3.));
#9554=CARTESIAN_POINT('Origin',(0.,0.,3.));
#9555=CARTESIAN_POINT('',(-2.59,-3.17183520979164E-16,3.25));
#9556=CARTESIAN_POINT('Origin',(0.,0.,3.25));
#9557=CARTESIAN_POINT('',(-2.59,-3.17183520979164E-16,3.));
#9558=CARTESIAN_POINT('',(-2.59,-3.17183520979164E-16,3.));
#9559=CARTESIAN_POINT('Origin',(0.,0.,3.));
#9560=CARTESIAN_POINT('Origin',(0.,0.,3.25));
#9561=CARTESIAN_POINT('',(-1.9,-2.32682891837997E-16,3.25));
#9562=CARTESIAN_POINT('Origin',(0.,0.,3.25));
#9563=CARTESIAN_POINT('Origin',(0.,0.,2.7));
#9564=CARTESIAN_POINT('',(-1.9,-2.32682891837997E-16,2.7));
#9565=CARTESIAN_POINT('',(-1.9,-2.32682891837997E-16,2.7));
#9566=CARTESIAN_POINT('Origin',(0.,0.,2.7));
#9567=CARTESIAN_POINT('Origin',(0.,0.,2.7));
#9568=CARTESIAN_POINT('',(-4.,-4.89858719658941E-16,3.));
#9569=CARTESIAN_POINT('Origin',(0.,0.,3.));
#9570=CARTESIAN_POINT('',(-4.,-4.89858719658941E-16,2.7));
#9571=CARTESIAN_POINT('',(-4.,-4.89858719658941E-16,2.7));
#9572=CARTESIAN_POINT('Origin',(0.,0.,2.7));
#9573=CARTESIAN_POINT('Origin',(0.,0.,3.));
#9574=CARTESIAN_POINT('Origin',(0.,0.,2.7));
#9575=CARTESIAN_POINT('',(0.,0.,0.));
#9576=CARTESIAN_POINT('Origin',(-6.95466594928129,-1.86349712473815,5.9));
#9577=CARTESIAN_POINT('',(-7.17966594928129,-1.86349712473815,6.));
#9578=CARTESIAN_POINT('Origin',(-6.95466594928129,-1.86349712473815,6.));
#9579=CARTESIAN_POINT('',(-7.17966594928129,-1.86349712473815,6.5));
#9580=CARTESIAN_POINT('',(-7.17966594928129,-1.86349712473815,5.9));
#9581=CARTESIAN_POINT('Origin',(-6.95466594928129,-1.86349712473815,6.5));
#9582=CARTESIAN_POINT('Origin',(-1.86349712473815,6.95466594928129,5.9));
#9583=CARTESIAN_POINT('',(-2.08849712473815,6.95466594928129,6.));
#9584=CARTESIAN_POINT('Origin',(-1.86349712473815,6.95466594928129,6.));
#9585=CARTESIAN_POINT('',(-2.08849712473815,6.95466594928129,6.5));
#9586=CARTESIAN_POINT('',(-2.08849712473815,6.95466594928129,5.9));
#9587=CARTESIAN_POINT('Origin',(-1.86349712473815,6.95466594928129,6.5));
#9588=CARTESIAN_POINT('Origin',(6.95466594928129,1.86349712473815,5.9));
#9589=CARTESIAN_POINT('',(6.72966594928129,1.86349712473815,6.));
#9590=CARTESIAN_POINT('Origin',(6.95466594928129,1.86349712473815,6.));
#9591=CARTESIAN_POINT('',(6.72966594928129,1.86349712473815,6.5));
#9592=CARTESIAN_POINT('',(6.72966594928129,1.86349712473815,5.9));
#9593=CARTESIAN_POINT('Origin',(6.95466594928129,1.86349712473815,6.5));
#9594=CARTESIAN_POINT('Origin',(1.86349712473815,-6.95466594928129,5.9));
#9595=CARTESIAN_POINT('',(1.63849712473815,-6.95466594928129,6.));
#9596=CARTESIAN_POINT('Origin',(1.86349712473815,-6.95466594928129,6.));
#9597=CARTESIAN_POINT('',(1.63849712473815,-6.95466594928129,6.5));
#9598=CARTESIAN_POINT('',(1.63849712473815,-6.95466594928129,5.9));
#9599=CARTESIAN_POINT('Origin',(1.86349712473815,-6.95466594928129,6.5));
#9600=CARTESIAN_POINT('Origin',(3.6,-6.23538290724796,5.9));
#9601=CARTESIAN_POINT('',(3.29,-6.23538290724796,6.));
#9602=CARTESIAN_POINT('Origin',(3.6,-6.23538290724796,6.));
#9603=CARTESIAN_POINT('',(3.29,-6.23538290724796,6.5));
#9604=CARTESIAN_POINT('',(3.29,-6.23538290724796,5.9));
#9605=CARTESIAN_POINT('Origin',(3.6,-6.23538290724796,6.5));
#9606=CARTESIAN_POINT('Origin',(-3.6,-6.23538290724796,5.9));
#9607=CARTESIAN_POINT('',(-3.91,-6.23538290724796,6.));
#9608=CARTESIAN_POINT('Origin',(-3.6,-6.23538290724796,6.));
#9609=CARTESIAN_POINT('',(-3.91,-6.23538290724796,6.5));
#9610=CARTESIAN_POINT('',(-3.91,-6.23538290724796,5.9));
#9611=CARTESIAN_POINT('Origin',(-3.6,-6.23538290724796,6.5));
#9612=CARTESIAN_POINT('Origin',(-7.2,8.81745695386094E-16,5.9));
#9613=CARTESIAN_POINT('',(-7.51,8.43781644612526E-16,6.));
#9614=CARTESIAN_POINT('Origin',(-7.2,8.81745695386094E-16,6.));
#9615=CARTESIAN_POINT('',(-7.51,9.19709746159662E-16,6.5));
#9616=CARTESIAN_POINT('',(-7.51,8.43781644612526E-16,5.9));
#9617=CARTESIAN_POINT('Origin',(-7.2,8.81745695386094E-16,6.5));
#9618=CARTESIAN_POINT('Origin',(-6.23538290724796,3.6,5.9));
#9619=CARTESIAN_POINT('',(-6.54538290724796,3.6,6.));
#9620=CARTESIAN_POINT('Origin',(-6.23538290724796,3.6,6.));
#9621=CARTESIAN_POINT('',(-6.54538290724796,3.6,6.5));
#9622=CARTESIAN_POINT('',(-6.54538290724796,3.6,5.9));
#9623=CARTESIAN_POINT('Origin',(-6.23538290724796,3.6,6.5));
#9624=CARTESIAN_POINT('Origin',(4.40872847693047E-16,7.2,5.9));
#9625=CARTESIAN_POINT('',(-0.31,7.2,6.));
#9626=CARTESIAN_POINT('Origin',(4.40872847693047E-16,7.2,6.));
#9627=CARTESIAN_POINT('',(-0.31,7.2,6.5));
#9628=CARTESIAN_POINT('',(-0.31,7.2,5.9));
#9629=CARTESIAN_POINT('Origin',(4.40872847693047E-16,7.2,6.5));
#9630=CARTESIAN_POINT('Origin',(6.23538290724796,3.6,5.9));
#9631=CARTESIAN_POINT('',(5.92538290724796,3.6,6.));
#9632=CARTESIAN_POINT('Origin',(6.23538290724796,3.6,6.));
#9633=CARTESIAN_POINT('',(5.92538290724796,3.6,6.5));
#9634=CARTESIAN_POINT('',(5.92538290724796,3.6,5.9));
#9635=CARTESIAN_POINT('Origin',(6.23538290724796,3.6,6.5));
#9636=CARTESIAN_POINT('Origin',(3.6,6.23538290724796,5.9));
#9637=CARTESIAN_POINT('',(3.29,6.23538290724796,6.));
#9638=CARTESIAN_POINT('Origin',(3.6,6.23538290724796,6.));
#9639=CARTESIAN_POINT('',(3.29,6.23538290724796,6.5));
#9640=CARTESIAN_POINT('',(3.29,6.23538290724796,5.9));
#9641=CARTESIAN_POINT('Origin',(3.6,6.23538290724796,6.5));
#9642=CARTESIAN_POINT('Origin',(-3.6,6.23538290724796,5.9));
#9643=CARTESIAN_POINT('',(-3.91,6.23538290724796,6.));
#9644=CARTESIAN_POINT('Origin',(-3.6,6.23538290724796,6.));
#9645=CARTESIAN_POINT('',(-3.91,6.23538290724796,6.5));
#9646=CARTESIAN_POINT('',(-3.91,6.23538290724796,5.9));
#9647=CARTESIAN_POINT('Origin',(-3.6,6.23538290724796,6.5));
#9648=CARTESIAN_POINT('Origin',(7.2,0.,5.9));
#9649=CARTESIAN_POINT('',(6.89,-3.79640507735679E-17,6.));
#9650=CARTESIAN_POINT('Origin',(7.2,0.,6.));
#9651=CARTESIAN_POINT('',(6.89,3.79640507735679E-17,6.5));
#9652=CARTESIAN_POINT('',(6.89,-3.79640507735679E-17,5.9));
#9653=CARTESIAN_POINT('Origin',(7.2,0.,6.5));
#9654=CARTESIAN_POINT('Origin',(-6.23538290724796,-3.6,5.9));
#9655=CARTESIAN_POINT('',(-6.54538290724796,-3.6,6.));
#9656=CARTESIAN_POINT('Origin',(-6.23538290724796,-3.6,6.));
#9657=CARTESIAN_POINT('',(-6.54538290724796,-3.6,6.5));
#9658=CARTESIAN_POINT('',(-6.54538290724796,-3.6,5.9));
#9659=CARTESIAN_POINT('Origin',(-6.23538290724796,-3.6,6.5));
#9660=CARTESIAN_POINT('Origin',(-1.32261854307914E-15,-7.2,5.9));
#9661=CARTESIAN_POINT('',(-0.310000000000001,-7.2,6.));
#9662=CARTESIAN_POINT('Origin',(-1.32261854307914E-15,-7.2,6.));
#9663=CARTESIAN_POINT('',(-0.310000000000001,-7.2,6.5));
#9664=CARTESIAN_POINT('',(-0.310000000000001,-7.2,5.9));
#9665=CARTESIAN_POINT('Origin',(-1.32261854307914E-15,-7.2,6.5));
#9666=CARTESIAN_POINT('Origin',(6.23538290724796,-3.6,5.9));
#9667=CARTESIAN_POINT('',(5.92538290724796,-3.6,6.));
#9668=CARTESIAN_POINT('Origin',(6.23538290724796,-3.6,6.));
#9669=CARTESIAN_POINT('',(5.92538290724796,-3.6,6.5));
#9670=CARTESIAN_POINT('',(5.92538290724796,-3.6,5.9));
#9671=CARTESIAN_POINT('Origin',(6.23538290724796,-3.6,6.5));
#9672=CARTESIAN_POINT('Origin',(0.,0.,6.));
#9673=CARTESIAN_POINT('',(-6.5,-7.9602041944578E-16,6.5));
#9674=CARTESIAN_POINT('Origin',(0.,0.,6.5));
#9675=CARTESIAN_POINT('',(-6.5,-7.9602041944578E-16,6.));
#9676=CARTESIAN_POINT('',(-6.5,-7.9602041944578E-16,6.));
#9677=CARTESIAN_POINT('Origin',(0.,0.,6.));
#9678=CARTESIAN_POINT('Origin',(0.,0.,6.));
#9679=CARTESIAN_POINT('',(-8.,-9.79717439317883E-16,6.5));
#9680=CARTESIAN_POINT('Origin',(0.,0.,6.5));
#9681=CARTESIAN_POINT('',(-8.,-9.79717439317883E-16,6.));
#9682=CARTESIAN_POINT('',(-8.,-9.79717439317883E-16,6.));
#9683=CARTESIAN_POINT('Origin',(0.,0.,6.));
#9684=CARTESIAN_POINT('Origin',(0.,0.,6.5));
#9685=CARTESIAN_POINT('Origin',(0.,0.,6.));
#9686=CARTESIAN_POINT('',(0.,0.,0.));
#9687=CARTESIAN_POINT('Origin',(0.3,0.4,0.));
#9688=CARTESIAN_POINT('',(-0.3,0.4,-3.67394039744206E-17));
#9689=CARTESIAN_POINT('Origin',(0.,0.4,0.));
#9690=CARTESIAN_POINT('Origin',(0.,0.375,0.));
#9691=CARTESIAN_POINT('',(-0.35,0.35,-4.28626379701573E-17));
#9692=CARTESIAN_POINT('Origin',(0.,0.35,0.));
#9693=CARTESIAN_POINT('',(-0.325,0.375,-3.9801020972289E-17));
#9694=CARTESIAN_POINT('Origin',(0.,0.19,0.));
#9695=CARTESIAN_POINT('',(-0.35,0.03,-4.28626379701574E-17));
#9696=CARTESIAN_POINT('Origin',(0.,0.03,0.));
#9697=CARTESIAN_POINT('',(-0.35,0.19,-4.28626379701574E-17));
#9698=CARTESIAN_POINT('Origin',(0.,0.0149999999999999,0.));
#9699=CARTESIAN_POINT('',(-0.32,-3.29597460435593E-17,-3.91886975727153E-17));
#9700=CARTESIAN_POINT('Origin',(0.,0.,0.));
#9701=CARTESIAN_POINT('',(-0.335,0.0149999999999999,-4.10256677714363E-17));
#9702=CARTESIAN_POINT('Origin',(0.22,0.,0.));
#9703=CARTESIAN_POINT('',(-0.22,-6.93889390390723E-18,-2.69422295812418E-17));
#9704=CARTESIAN_POINT('Origin',(0.,0.,0.));
#9705=CARTESIAN_POINT('Origin',(0.,-0.02,0.));
#9706=CARTESIAN_POINT('',(-0.1954,-0.0492,2.39295984553393E-17));
#9707=CARTESIAN_POINT('Origin',(0.,-0.0492,0.));
#9708=CARTESIAN_POINT('',(-0.21,-0.02,-2.57175827820944E-17));
#9709=CARTESIAN_POINT('Origin',(0.,-0.8,0.));
#9710=CARTESIAN_POINT('',(-0.1954,-1.5646,2.39295984553393E-17));
#9711=CARTESIAN_POINT('Origin',(0.,-1.5646,0.));
#9712=CARTESIAN_POINT('',(-0.1954,-0.8,-2.39295984553393E-17));
#9713=CARTESIAN_POINT('Origin',(0.,-1.58,0.));
#9714=CARTESIAN_POINT('',(-0.16,-1.6,-1.95943487863577E-17));
#9715=CARTESIAN_POINT('Origin',(0.,-1.6,0.));
#9716=CARTESIAN_POINT('',(-0.18,-1.58,-2.20436423846524E-17));
#9717=CARTESIAN_POINT('Origin',(0.,-1.6,0.));
#9718=CARTESIAN_POINT('Origin',(0.0866025403784439,-0.4,-0.15));
#9719=CARTESIAN_POINT('',(0.173205080756888,-0.4,0.));
#9720=CARTESIAN_POINT('',(0.0866025403784439,-0.4,-0.15));
#9721=CARTESIAN_POINT('',(0.173205080756888,-0.4,0.));
#9722=CARTESIAN_POINT('',(0.0866025403784439,-0.64,-0.15));
#9723=CARTESIAN_POINT('',(0.0866025403784439,-0.4,-0.15));
#9724=CARTESIAN_POINT('',(0.173205080756888,-0.64,0.));
#9725=CARTESIAN_POINT('',(0.173205080756888,-0.64,0.));
#9726=CARTESIAN_POINT('',(0.173205080756888,-0.4,0.));
#9727=CARTESIAN_POINT('Origin',(-0.0866025403784438,-0.4,-0.15));
#9728=CARTESIAN_POINT('',(-0.0866025403784438,-0.4,-0.15));
#9729=CARTESIAN_POINT('',(0.0866025403784439,-0.4,-0.15));
#9730=CARTESIAN_POINT('',(-0.0866025403784438,-0.64,-0.15));
#9731=CARTESIAN_POINT('',(-0.0866025403784438,-0.4,-0.15));
#9732=CARTESIAN_POINT('',(0.0866025403784439,-0.64,-0.15));
#9733=CARTESIAN_POINT('Origin',(-0.173205080756888,-0.4,-2.77555756156289E-17));
#9734=CARTESIAN_POINT('',(-0.173205080756888,-0.4,-2.12115047744981E-17));
#9735=CARTESIAN_POINT('',(-0.0866025403784438,-0.4,-0.15));
#9736=CARTESIAN_POINT('',(-0.173205080756888,-0.64,-2.77555756156289E-17));
#9737=CARTESIAN_POINT('',(-0.173205080756888,-0.4,-2.12115047744981E-17));
#9738=CARTESIAN_POINT('',(-0.0866025403784438,-0.64,-0.15));
#9739=CARTESIAN_POINT('Origin',(-0.0866025403784439,-0.4,0.15));
#9740=CARTESIAN_POINT('',(-0.0866025403784439,-0.4,0.15));
#9741=CARTESIAN_POINT('',(-0.173205080756888,-0.4,-2.12115047744981E-17));
#9742=CARTESIAN_POINT('',(-0.0866025403784439,-0.64,0.15));
#9743=CARTESIAN_POINT('',(-0.0866025403784439,-0.4,0.15));
#9744=CARTESIAN_POINT('',(-0.173205080756888,-0.64,-2.12115047744981E-17));
#9745=CARTESIAN_POINT('Origin',(0.0866025403784439,-0.4,0.15));
#9746=CARTESIAN_POINT('',(0.0866025403784439,-0.4,0.15));
#9747=CARTESIAN_POINT('',(-0.0866025403784439,-0.4,0.15));
#9748=CARTESIAN_POINT('',(0.0866025403784439,-0.64,0.15));
#9749=CARTESIAN_POINT('',(0.0866025403784439,-0.4,0.15));
#9750=CARTESIAN_POINT('',(-0.0866025403784439,-0.64,0.15));
#9751=CARTESIAN_POINT('Origin',(0.173205080756888,-0.4,0.));
#9752=CARTESIAN_POINT('',(0.0866025403784439,-0.4,0.15));
#9753=CARTESIAN_POINT('',(0.0866025403784439,-0.64,0.15));
#9754=CARTESIAN_POINT('Origin',(0.,-0.4,-2.77555756156289E-17));
#9755=CARTESIAN_POINT('Origin',(0.,-0.64,-2.77555756156289E-17));
#9756=CARTESIAN_POINT('',(0.,0.,0.));
#9757=CARTESIAN_POINT('',(0.,0.,0.));
#9758=CARTESIAN_POINT('',(0.,0.,0.));
#9759=CARTESIAN_POINT('',(0.,0.,0.));
#9760=CARTESIAN_POINT('',(0.,0.,0.));
#9761=CARTESIAN_POINT('',(0.,0.,0.));
#9762=CARTESIAN_POINT('',(0.,0.,0.));
#9763=CARTESIAN_POINT('',(0.,0.,0.));
#9764=CARTESIAN_POINT('',(0.,0.,0.));
#9765=CARTESIAN_POINT('',(0.,0.,0.));
#9766=CARTESIAN_POINT('',(0.,0.,0.));
#9767=CARTESIAN_POINT('',(1.90918830920368,1.90918830920368,0.8));
#9768=CARTESIAN_POINT('',(1.90918830920368,1.90918830920368,0.96));
#9769=CARTESIAN_POINT('',(-1.90918830920368,1.90918830920368,0.8));
#9770=CARTESIAN_POINT('',(-1.90918830920368,1.90918830920368,0.96));
#9771=CARTESIAN_POINT('',(-1.90918830920368,-1.90918830920368,0.8));
#9772=CARTESIAN_POINT('',(-1.90918830920368,-1.90918830920368,0.96));
#9773=CARTESIAN_POINT('',(1.90918830920368,-1.90918830920368,0.8));
#9774=CARTESIAN_POINT('',(1.90918830920368,-1.90918830920368,0.96));
#9775=CARTESIAN_POINT('',(0.,0.,4.));
#9776=CARTESIAN_POINT('',(1.75,0.,6.6));
#9777=CARTESIAN_POINT('',(7.2,1.6,1.));
#9778=CARTESIAN_POINT('',(7.2,-1.6,1.));
#9779=CARTESIAN_POINT('',(0.,0.,0.));
#9780=CARTESIAN_POINT('',(0.,0.,0.));
#9781=CARTESIAN_POINT('',(0.,0.,0.));
#9782=CARTESIAN_POINT('',(0.,0.,0.));
#9783=CARTESIAN_POINT('',(2.33345237791561,2.33345237791561,2.7));
#9784=CARTESIAN_POINT('',(-2.33345237791561,2.33345237791561,2.7));
#9785=CARTESIAN_POINT('',(-2.33345237791561,-2.33345237791561,2.7));
#9786=CARTESIAN_POINT('',(2.33345237791561,-2.33345237791561,2.7));
#9787=CARTESIAN_POINT('',(6.95466594928129,1.86349712473815,6.));
#9788=CARTESIAN_POINT('',(-1.86349712473815,6.95466594928129,6.));
#9789=CARTESIAN_POINT('',(-6.95466594928129,-1.86349712473815,6.));
#9790=CARTESIAN_POINT('',(1.86349712473815,-6.95466594928129,6.));
#9791=CARTESIAN_POINT('',(0.,0.,0.));
#9792=CARTESIAN_POINT('',(0.,0.,0.));
#9793=CARTESIAN_POINT('Origin',(7.2,0.,-3.));
#9794=CARTESIAN_POINT('',(6.9,-3.67394039744206E-17,-3.));
#9795=CARTESIAN_POINT('Origin',(7.2,0.,-3.));
#9796=CARTESIAN_POINT('Origin',(7.2,0.,4.8));
#9797=CARTESIAN_POINT('',(6.7,-6.12323399573677E-17,4.8));
#9798=CARTESIAN_POINT('Origin',(7.2,0.,4.8));
#9799=CARTESIAN_POINT('',(6.9,-3.67394039744206E-17,4.8));
#9800=CARTESIAN_POINT('Origin',(7.2,0.,4.8));
#9801=CARTESIAN_POINT('Origin',(7.2,0.,4.5));
#9802=CARTESIAN_POINT('',(6.7,-6.12323399573677E-17,4.5));
#9803=CARTESIAN_POINT('Origin',(7.2,0.,4.5));
#9804=CARTESIAN_POINT('',(6.9,3.67394039744206E-17,4.5));
#9805=CARTESIAN_POINT('Origin',(7.2,0.,4.5));
#9806=CARTESIAN_POINT('Origin',(7.2,0.,4.5));
#9807=CARTESIAN_POINT('',(6.7,-6.12323399573677E-17,4.5));
#9808=CARTESIAN_POINT('Origin',(7.2,0.,-1.5));
#9809=CARTESIAN_POINT('',(6.9,-3.67394039744206E-17,-1.5));
#9810=CARTESIAN_POINT('Origin',(7.2,0.,-1.5));
#9811=CARTESIAN_POINT('',(6.9,-3.67394039744206E-17,7.));
#9812=CARTESIAN_POINT('Origin',(7.2,0.,7.));
#9813=CARTESIAN_POINT('',(6.9,-3.67394039744206E-17,-1.5));
#9814=CARTESIAN_POINT('Origin',(7.2,0.,7.));
#9815=CARTESIAN_POINT('',(0.,0.,0.));
#9816=CARTESIAN_POINT('Origin',(7.49,0.,-2.2));
#9817=CARTESIAN_POINT('',(7.49,0.0768114574786819,-2.39544820285692));
#9818=CARTESIAN_POINT('',(7.49,0.0768114574786819,-2.00455179714308));
#9819=CARTESIAN_POINT('',(7.49,0.0768114574786819,-3.));
#9820=CARTESIAN_POINT('Origin',(7.49,0.,-2.2));
#9821=CARTESIAN_POINT('Origin',(7.49,0.,-2.2));
#9822=CARTESIAN_POINT('',(7.49,-0.0768114574786819,-2.39544820285692));
#9823=CARTESIAN_POINT('Ctrl Pts',(7.49,-0.0768114574786819,-2.39544820285692));
#9824=CARTESIAN_POINT('Ctrl Pts',(7.49646752117291,-0.0523934708695169,
-2.40504451079288));
#9825=CARTESIAN_POINT('Ctrl Pts',(7.5,-0.025670625777551,-2.41));
#9826=CARTESIAN_POINT('Ctrl Pts',(7.5,0.025670625777551,-2.41));
#9827=CARTESIAN_POINT('Ctrl Pts',(7.49646752117291,0.0523934708695169,-2.40504451079288));
#9828=CARTESIAN_POINT('Ctrl Pts',(7.49,0.0768114574786818,-2.39544820285692));
#9829=CARTESIAN_POINT('',(7.49,-0.0768114574786819,-2.00455179714308));
#9830=CARTESIAN_POINT('Origin',(7.49,0.,-2.2));
#9831=CARTESIAN_POINT('',(7.5,-1.63282383430008E-17,-1.99));
#9832=CARTESIAN_POINT('Ctrl Pts',(7.5,-3.46944695195361E-18,-1.99));
#9833=CARTESIAN_POINT('Ctrl Pts',(7.5,-0.0256706257775511,-1.99));
#9834=CARTESIAN_POINT('Ctrl Pts',(7.49646752117291,-0.0523934708695168,
-1.99495548920712));
#9835=CARTESIAN_POINT('Ctrl Pts',(7.49,-0.0768114574786816,-2.00455179714308));
#9836=CARTESIAN_POINT('',(8.4,-2.57175827820944E-17,-1.99));
#9837=CARTESIAN_POINT('',(7.49,-2.57175827820944E-17,-1.99));
#9838=CARTESIAN_POINT('',(8.38148212005091,0.21,-2.2));
#9839=CARTESIAN_POINT('Ctrl Pts',(8.38148212005091,0.21,-2.2));
#9840=CARTESIAN_POINT('Ctrl Pts',(8.38148212005091,0.21,-2.22642707101426));
#9841=CARTESIAN_POINT('Ctrl Pts',(8.38246056146673,0.204707379175836,-2.25457755408867));
#9842=CARTESIAN_POINT('Ctrl Pts',(8.38597389417424,0.183259409780014,-2.30630056955556));
#9843=CARTESIAN_POINT('Ctrl Pts',(8.38845578531258,0.167106958412512,-2.32987788968584));
#9844=CARTESIAN_POINT('Ctrl Pts',(8.3930982535617,0.129878495645339,-2.36710635245301));
#9845=CARTESIAN_POINT('Ctrl Pts',(8.39556345497295,0.106300916040875,-2.38325927901602));
#9846=CARTESIAN_POINT('Ctrl Pts',(8.39903845223025,0.0545770066794469,-2.40470759325685));
#9847=CARTESIAN_POINT('Ctrl Pts',(8.4,0.0264262107330192,-2.41));
#9848=CARTESIAN_POINT('Ctrl Pts',(8.4,-0.0264262107330192,-2.41));
#9849=CARTESIAN_POINT('Ctrl Pts',(8.39903845223025,-0.0545770066794469,
-2.40470759325685));
#9850=CARTESIAN_POINT('Ctrl Pts',(8.39556345497295,-0.106300916040875,-2.38325927901602));
#9851=CARTESIAN_POINT('Ctrl Pts',(8.3930982535617,-0.129878495645339,-2.36710635245301));
#9852=CARTESIAN_POINT('Ctrl Pts',(8.38845578531258,-0.167106958412512,-2.32987788968584));
#9853=CARTESIAN_POINT('Ctrl Pts',(8.38597389417424,-0.183259409780014,-2.30630056955556));
#9854=CARTESIAN_POINT('Ctrl Pts',(8.38246056146673,-0.204707379175836,-2.25457755408867));
#9855=CARTESIAN_POINT('Ctrl Pts',(8.38148212005091,-0.21,-2.22642707101426));
#9856=CARTESIAN_POINT('Ctrl Pts',(8.38148212005091,-0.21,-2.17357292898574));
#9857=CARTESIAN_POINT('Ctrl Pts',(8.38246056146673,-0.204707379175836,-2.14542244591133));
#9858=CARTESIAN_POINT('Ctrl Pts',(8.38597389417424,-0.183259409780014,-2.09369943044444));
#9859=CARTESIAN_POINT('Ctrl Pts',(8.38845578531258,-0.167106958412512,-2.07012211031416));
#9860=CARTESIAN_POINT('Ctrl Pts',(8.3930982535617,-0.129878495645339,-2.03289364754699));
#9861=CARTESIAN_POINT('Ctrl Pts',(8.39556345497295,-0.106300916040875,-2.01674072098398));
#9862=CARTESIAN_POINT('Ctrl Pts',(8.39903845223025,-0.0545770066794469,
-1.99529240674315));
#9863=CARTESIAN_POINT('Ctrl Pts',(8.4,-0.0264262107330192,-1.99));
#9864=CARTESIAN_POINT('Ctrl Pts',(8.4,-4.85722573273506E-17,-1.99));
#9865=CARTESIAN_POINT('Ctrl Pts',(8.4,-8.32667268468867E-17,-1.99));
#9866=CARTESIAN_POINT('Ctrl Pts',(8.4,0.0264262107330192,-1.99));
#9867=CARTESIAN_POINT('Ctrl Pts',(8.39903845223025,0.0545770066794466,-1.99529240674315));
#9868=CARTESIAN_POINT('Ctrl Pts',(8.39556345497295,0.106300916040875,-2.01674072098398));
#9869=CARTESIAN_POINT('Ctrl Pts',(8.3930982535617,0.129878495645339,-2.03289364754699));
#9870=CARTESIAN_POINT('Ctrl Pts',(8.38845578531258,0.167106958412512,-2.07012211031416));
#9871=CARTESIAN_POINT('Ctrl Pts',(8.38597389417424,0.183259409780014,-2.09369943044444));
#9872=CARTESIAN_POINT('Ctrl Pts',(8.38246056146673,0.204707379175836,-2.14542244591133));
#9873=CARTESIAN_POINT('Ctrl Pts',(8.38148212005091,0.21,-2.17357292898574));
#9874=CARTESIAN_POINT('Ctrl Pts',(8.38148212005091,0.21,-2.2));
#9875=CARTESIAN_POINT('Ctrl Pts',(7.49,0.0768114574786816,-2.00455179714308));
#9876=CARTESIAN_POINT('Ctrl Pts',(7.49646752117291,0.0523934708695167,-1.99495548920712));
#9877=CARTESIAN_POINT('Ctrl Pts',(7.5,0.025670625777551,-1.99));
#9878=CARTESIAN_POINT('Ctrl Pts',(7.5,-5.55111512312578E-17,-1.99));
#9879=CARTESIAN_POINT('Origin',(7.49,0.,-2.2));
#9880=CARTESIAN_POINT('',(7.49,-0.0768114574786819,-3.));
#9881=CARTESIAN_POINT('Origin',(7.2,0.,-3.));
#9882=CARTESIAN_POINT('',(6.9,-3.67394039744206E-17,-1.5));
#9883=CARTESIAN_POINT('Origin',(7.2,0.,-1.5));
#9884=CARTESIAN_POINT('',(6.9,-3.67394039744206E-17,-3.));
#9885=CARTESIAN_POINT('',(6.9,-3.67394039744206E-17,-3.));
#9886=CARTESIAN_POINT('Origin',(7.2,0.,-3.));
#9887=CARTESIAN_POINT('Origin',(7.2,0.,-3.));
#9888=CARTESIAN_POINT('',(6.,-1.46957615897682E-16,-1.5));
#9889=CARTESIAN_POINT('Origin',(7.2,0.,-1.5));
#9890=CARTESIAN_POINT('',(6.,-1.46957615897682E-16,-3.));
#9891=CARTESIAN_POINT('',(6.,-1.46957615897682E-16,-3.));
#9892=CARTESIAN_POINT('Origin',(7.2,0.,-3.));
#9893=CARTESIAN_POINT('Origin',(7.2,0.,-1.5));
#9894=CARTESIAN_POINT('Origin',(7.2,0.,-3.));
#9895=CARTESIAN_POINT('',(0.,0.,0.));
#9896=CARTESIAN_POINT('Origin',(0.0721687836487032,0.,-0.125));
#9897=CARTESIAN_POINT('',(0.0721687836487032,0.,-0.125));
#9898=CARTESIAN_POINT('',(0.144337567297406,0.,0.));
#9899=CARTESIAN_POINT('',(0.117710979560879,0.,-0.0461186027918559));
#9900=CARTESIAN_POINT('',(0.0721687836487032,-0.25,-0.125));
#9901=CARTESIAN_POINT('',(0.0721687836487032,0.,-0.125));
#9902=CARTESIAN_POINT('',(0.144337567297406,-0.25,0.));
#9903=CARTESIAN_POINT('',(0.144337567297406,-0.25,0.));
#9904=CARTESIAN_POINT('',(0.144337567297406,0.,0.));
#9905=CARTESIAN_POINT('Origin',(-0.0721687836487032,0.,-0.125));
#9906=CARTESIAN_POINT('',(-0.0721687836487032,0.,-0.125));
#9907=CARTESIAN_POINT('',(0.0739156081756484,0.,-0.125));
#9908=CARTESIAN_POINT('',(-0.0721687836487032,-0.25,-0.125));
#9909=CARTESIAN_POINT('',(-0.0721687836487032,0.,-0.125));
#9910=CARTESIAN_POINT('',(0.0721687836487032,-0.25,-0.125));
#9911=CARTESIAN_POINT('Origin',(-0.144337567297406,0.,-4.16333634234434E-17));
#9912=CARTESIAN_POINT('',(-0.144337567297406,0.,-1.76762539787485E-17));
#9913=CARTESIAN_POINT('',(-0.0987953713852306,0.,-0.0788813972081442));
#9914=CARTESIAN_POINT('',(-0.144337567297406,-0.25,-2.77555756156289E-17));
#9915=CARTESIAN_POINT('',(-0.144337567297406,0.,-1.76762539787485E-17));
#9916=CARTESIAN_POINT('',(-0.0721687836487032,-0.25,-0.125));
#9917=CARTESIAN_POINT('Origin',(-0.0721687836487033,0.,0.125));
#9918=CARTESIAN_POINT('',(-0.0721687836487033,0.,0.125));
#9919=CARTESIAN_POINT('',(-0.0627109795608791,0.,0.141381397208144));
#9920=CARTESIAN_POINT('',(-0.0721687836487033,-0.25,0.125));
#9921=CARTESIAN_POINT('',(-0.0721687836487033,0.,0.125));
#9922=CARTESIAN_POINT('',(-0.144337567297406,-0.25,-1.76762539787485E-17));
#9923=CARTESIAN_POINT('Origin',(0.0721687836487032,0.,0.125));
#9924=CARTESIAN_POINT('',(0.0721687836487032,0.,0.125));
#9925=CARTESIAN_POINT('',(0.146084391824352,0.,0.125));
#9926=CARTESIAN_POINT('',(0.0721687836487032,-0.25,0.125));
#9927=CARTESIAN_POINT('',(0.0721687836487032,0.,0.125));
#9928=CARTESIAN_POINT('',(-0.0721687836487033,-0.25,0.125));
#9929=CARTESIAN_POINT('Origin',(0.144337567297406,0.,0.));
#9930=CARTESIAN_POINT('',(0.153795371385231,0.,-0.0163813972081441));
#9931=CARTESIAN_POINT('',(0.0721687836487032,-0.25,0.125));
#9932=CARTESIAN_POINT('Origin',(0.,-0.25,0.));
#9933=CARTESIAN_POINT('Origin',(0.22,0.,0.));
#9934=CARTESIAN_POINT('',(-0.22,-8.67361737988404E-18,-2.69422295812418E-17));
#9935=CARTESIAN_POINT('Origin',(0.,0.,0.));
#9936=CARTESIAN_POINT('Origin',(0.,-0.015,0.));
#9937=CARTESIAN_POINT('',(-0.24505,-0.02505,-3.00099698131059E-17));
#9938=CARTESIAN_POINT('Origin',(0.,-0.02505,0.));
#9939=CARTESIAN_POINT('',(-0.235,-0.015,-2.87791997799628E-17));
#9940=CARTESIAN_POINT('Origin',(0.,-0.3775,0.));
#9941=CARTESIAN_POINT('',(-0.24505,-0.72995,3.00099698131059E-17));
#9942=CARTESIAN_POINT('Origin',(0.,-0.72995,0.));
#9943=CARTESIAN_POINT('',(-0.24505,-0.3775,-3.00099698131059E-17));
#9944=CARTESIAN_POINT('Origin',(0.,-0.7625,0.));
#9945=CARTESIAN_POINT('',(-0.175,-0.8,-2.14313189850787E-17));
#9946=CARTESIAN_POINT('Origin',(0.,-0.8,0.));
#9947=CARTESIAN_POINT('',(-0.2125,-0.7625,-2.60237444818813E-17));
#9948=CARTESIAN_POINT('Origin',(0.,-0.8,0.));
#9949=CARTESIAN_POINT('',(0.,0.,0.));
#9950=CARTESIAN_POINT('',(0.,0.,0.));
#9951=CARTESIAN_POINT('',(8.3,0.,-2.2));
#9952=CARTESIAN_POINT('',(0.,0.,0.));
#9953=CARTESIAN_POINT('',(0.,0.,0.));
#9954=CARTESIAN_POINT('',(0.,0.,0.));
#9955=UNCERTAINTY_MEASURE_WITH_UNIT(LENGTH_MEASURE(0.001),#10021,
'DISTANCE_ACCURACY_VALUE',
'Maximum model space distance between geometric entities at asserted c
onnectivities');
#9956=UNCERTAINTY_MEASURE_WITH_UNIT(LENGTH_MEASURE(0.001),#10021,
'DISTANCE_ACCURACY_VALUE',
'Maximum model space distance between geometric entities at asserted c
onnectivities');
#9957=UNCERTAINTY_MEASURE_WITH_UNIT(LENGTH_MEASURE(0.001),#10021,
'DISTANCE_ACCURACY_VALUE',
'Maximum model space distance between geometric entities at asserted c
onnectivities');
#9958=UNCERTAINTY_MEASURE_WITH_UNIT(LENGTH_MEASURE(0.001),#10021,
'DISTANCE_ACCURACY_VALUE',
'Maximum model space distance between geometric entities at asserted c
onnectivities');
#9959=UNCERTAINTY_MEASURE_WITH_UNIT(LENGTH_MEASURE(0.001),#10021,
'DISTANCE_ACCURACY_VALUE',
'Maximum model space distance between geometric entities at asserted c
onnectivities');
#9960=UNCERTAINTY_MEASURE_WITH_UNIT(LENGTH_MEASURE(0.001),#10021,
'DISTANCE_ACCURACY_VALUE',
'Maximum model space distance between geometric entities at asserted c
onnectivities');
#9961=UNCERTAINTY_MEASURE_WITH_UNIT(LENGTH_MEASURE(0.001),#10021,
'DISTANCE_ACCURACY_VALUE',
'Maximum model space distance between geometric entities at asserted c
onnectivities');
#9962=UNCERTAINTY_MEASURE_WITH_UNIT(LENGTH_MEASURE(0.001),#10021,
'DISTANCE_ACCURACY_VALUE',
'Maximum model space distance between geometric entities at asserted c
onnectivities');
#9963=UNCERTAINTY_MEASURE_WITH_UNIT(LENGTH_MEASURE(0.001),#10021,
'DISTANCE_ACCURACY_VALUE',
'Maximum model space distance between geometric entities at asserted c
onnectivities');
#9964=UNCERTAINTY_MEASURE_WITH_UNIT(LENGTH_MEASURE(0.001),#10021,
'DISTANCE_ACCURACY_VALUE',
'Maximum model space distance between geometric entities at asserted c
onnectivities');
#9965=UNCERTAINTY_MEASURE_WITH_UNIT(LENGTH_MEASURE(0.001),#10021,
'DISTANCE_ACCURACY_VALUE',
'Maximum model space distance between geometric entities at asserted c
onnectivities');
#9966=UNCERTAINTY_MEASURE_WITH_UNIT(LENGTH_MEASURE(0.001),#10021,
'DISTANCE_ACCURACY_VALUE',
'Maximum model space distance between geometric entities at asserted c
onnectivities');
#9967=UNCERTAINTY_MEASURE_WITH_UNIT(LENGTH_MEASURE(0.001),#10021,
'DISTANCE_ACCURACY_VALUE',
'Maximum model space distance between geometric entities at asserted c
onnectivities');
#9968=UNCERTAINTY_MEASURE_WITH_UNIT(LENGTH_MEASURE(0.001),#10021,
'DISTANCE_ACCURACY_VALUE',
'Maximum model space distance between geometric entities at asserted c
onnectivities');
#9969=UNCERTAINTY_MEASURE_WITH_UNIT(LENGTH_MEASURE(0.001),#10021,
'DISTANCE_ACCURACY_VALUE',
'Maximum model space distance between geometric entities at asserted c
onnectivities');
#9970=UNCERTAINTY_MEASURE_WITH_UNIT(LENGTH_MEASURE(0.001),#10021,
'DISTANCE_ACCURACY_VALUE',
'Maximum model space distance between geometric entities at asserted c
onnectivities');
#9971=UNCERTAINTY_MEASURE_WITH_UNIT(LENGTH_MEASURE(0.001),#10021,
'DISTANCE_ACCURACY_VALUE',
'Maximum model space distance between geometric entities at asserted c
onnectivities');
#9972=UNCERTAINTY_MEASURE_WITH_UNIT(LENGTH_MEASURE(0.001),#10021,
'DISTANCE_ACCURACY_VALUE',
'Maximum model space distance between geometric entities at asserted c
onnectivities');
#9973=UNCERTAINTY_MEASURE_WITH_UNIT(LENGTH_MEASURE(0.001),#10021,
'DISTANCE_ACCURACY_VALUE',
'Maximum model space distance between geometric entities at asserted c
onnectivities');
#9974=UNCERTAINTY_MEASURE_WITH_UNIT(LENGTH_MEASURE(0.001),#10021,
'DISTANCE_ACCURACY_VALUE',
'Maximum model space distance between geometric entities at asserted c
onnectivities');
#9975=UNCERTAINTY_MEASURE_WITH_UNIT(LENGTH_MEASURE(0.001),#10021,
'DISTANCE_ACCURACY_VALUE',
'Maximum model space distance between geometric entities at asserted c
onnectivities');
#9976=UNCERTAINTY_MEASURE_WITH_UNIT(LENGTH_MEASURE(0.001),#10021,
'DISTANCE_ACCURACY_VALUE',
'Maximum model space distance between geometric entities at asserted c
onnectivities');
#9977=UNCERTAINTY_MEASURE_WITH_UNIT(LENGTH_MEASURE(0.001),#10021,
'DISTANCE_ACCURACY_VALUE',
'Maximum model space distance between geometric entities at asserted c
onnectivities');
#9978=UNCERTAINTY_MEASURE_WITH_UNIT(LENGTH_MEASURE(0.001),#10021,
'DISTANCE_ACCURACY_VALUE',
'Maximum model space distance between geometric entities at asserted c
onnectivities');
#9979=UNCERTAINTY_MEASURE_WITH_UNIT(LENGTH_MEASURE(0.001),#10021,
'DISTANCE_ACCURACY_VALUE',
'Maximum model space distance between geometric entities at asserted c
onnectivities');
#9980=UNCERTAINTY_MEASURE_WITH_UNIT(LENGTH_MEASURE(0.001),#10021,
'DISTANCE_ACCURACY_VALUE',
'Maximum model space distance between geometric entities at asserted c
onnectivities');
#9981=UNCERTAINTY_MEASURE_WITH_UNIT(LENGTH_MEASURE(0.001),#10021,
'DISTANCE_ACCURACY_VALUE',
'Maximum model space distance between geometric entities at asserted c
onnectivities');
#9982=UNCERTAINTY_MEASURE_WITH_UNIT(LENGTH_MEASURE(0.001),#10021,
'DISTANCE_ACCURACY_VALUE',
'Maximum model space distance between geometric entities at asserted c
onnectivities');
#9983=UNCERTAINTY_MEASURE_WITH_UNIT(LENGTH_MEASURE(0.001),#10021,
'DISTANCE_ACCURACY_VALUE',
'Maximum model space distance between geometric entities at asserted c
onnectivities');
#9984=UNCERTAINTY_MEASURE_WITH_UNIT(LENGTH_MEASURE(0.001),#10021,
'DISTANCE_ACCURACY_VALUE',
'Maximum model space distance between geometric entities at asserted c
onnectivities');
#9985=UNCERTAINTY_MEASURE_WITH_UNIT(LENGTH_MEASURE(0.001),#10021,
'DISTANCE_ACCURACY_VALUE',
'Maximum model space distance between geometric entities at asserted c
onnectivities');
#9986=UNCERTAINTY_MEASURE_WITH_UNIT(LENGTH_MEASURE(0.001),#10021,
'DISTANCE_ACCURACY_VALUE',
'Maximum model space distance between geometric entities at asserted c
onnectivities');
#9987=UNCERTAINTY_MEASURE_WITH_UNIT(LENGTH_MEASURE(0.001),#10021,
'DISTANCE_ACCURACY_VALUE',
'Maximum model space distance between geometric entities at asserted c
onnectivities');
#9988=(
GEOMETRIC_REPRESENTATION_CONTEXT(3)
GLOBAL_UNCERTAINTY_ASSIGNED_CONTEXT((#9955))
GLOBAL_UNIT_ASSIGNED_CONTEXT((#10021,#10023,#10024))
REPRESENTATION_CONTEXT('','3D')
);
#9989=(
GEOMETRIC_REPRESENTATION_CONTEXT(3)
GLOBAL_UNCERTAINTY_ASSIGNED_CONTEXT((#9956))
GLOBAL_UNIT_ASSIGNED_CONTEXT((#10021,#10023,#10024))
REPRESENTATION_CONTEXT('','3D')
);
#9990=(
GEOMETRIC_REPRESENTATION_CONTEXT(3)
GLOBAL_UNCERTAINTY_ASSIGNED_CONTEXT((#9957))
GLOBAL_UNIT_ASSIGNED_CONTEXT((#10021,#10023,#10024))
REPRESENTATION_CONTEXT('','3D')
);
#9991=(
GEOMETRIC_REPRESENTATION_CONTEXT(3)
GLOBAL_UNCERTAINTY_ASSIGNED_CONTEXT((#9958))
GLOBAL_UNIT_ASSIGNED_CONTEXT((#10021,#10023,#10024))
REPRESENTATION_CONTEXT('','3D')
);
#9992=(
GEOMETRIC_REPRESENTATION_CONTEXT(3)
GLOBAL_UNCERTAINTY_ASSIGNED_CONTEXT((#9959))
GLOBAL_UNIT_ASSIGNED_CONTEXT((#10021,#10023,#10024))
REPRESENTATION_CONTEXT('','3D')
);
#9993=(
GEOMETRIC_REPRESENTATION_CONTEXT(3)
GLOBAL_UNCERTAINTY_ASSIGNED_CONTEXT((#9960))
GLOBAL_UNIT_ASSIGNED_CONTEXT((#10021,#10023,#10024))
REPRESENTATION_CONTEXT('','3D')
);
#9994=(
GEOMETRIC_REPRESENTATION_CONTEXT(3)
GLOBAL_UNCERTAINTY_ASSIGNED_CONTEXT((#9961))
GLOBAL_UNIT_ASSIGNED_CONTEXT((#10021,#10023,#10024))
REPRESENTATION_CONTEXT('','3D')
);
#9995=(
GEOMETRIC_REPRESENTATION_CONTEXT(3)
GLOBAL_UNCERTAINTY_ASSIGNED_CONTEXT((#9962))
GLOBAL_UNIT_ASSIGNED_CONTEXT((#10021,#10023,#10024))
REPRESENTATION_CONTEXT('','3D')
);
#9996=(
GEOMETRIC_REPRESENTATION_CONTEXT(3)
GLOBAL_UNCERTAINTY_ASSIGNED_CONTEXT((#9963))
GLOBAL_UNIT_ASSIGNED_CONTEXT((#10021,#10023,#10024))
REPRESENTATION_CONTEXT('','3D')
);
#9997=(
GEOMETRIC_REPRESENTATION_CONTEXT(3)
GLOBAL_UNCERTAINTY_ASSIGNED_CONTEXT((#9964))
GLOBAL_UNIT_ASSIGNED_CONTEXT((#10021,#10023,#10024))
REPRESENTATION_CONTEXT('','3D')
);
#9998=(
GEOMETRIC_REPRESENTATION_CONTEXT(3)
GLOBAL_UNCERTAINTY_ASSIGNED_CONTEXT((#9965))
GLOBAL_UNIT_ASSIGNED_CONTEXT((#10021,#10023,#10024))
REPRESENTATION_CONTEXT('','3D')
);
#9999=(
GEOMETRIC_REPRESENTATION_CONTEXT(3)
GLOBAL_UNCERTAINTY_ASSIGNED_CONTEXT((#9966))
GLOBAL_UNIT_ASSIGNED_CONTEXT((#10021,#10023,#10024))
REPRESENTATION_CONTEXT('','3D')
);
#10000=(
GEOMETRIC_REPRESENTATION_CONTEXT(3)
GLOBAL_UNCERTAINTY_ASSIGNED_CONTEXT((#9967))
GLOBAL_UNIT_ASSIGNED_CONTEXT((#10021,#10023,#10024))
REPRESENTATION_CONTEXT('','3D')
);
#10001=(
GEOMETRIC_REPRESENTATION_CONTEXT(3)
GLOBAL_UNCERTAINTY_ASSIGNED_CONTEXT((#9968))
GLOBAL_UNIT_ASSIGNED_CONTEXT((#10021,#10023,#10024))
REPRESENTATION_CONTEXT('','3D')
);
#10002=(
GEOMETRIC_REPRESENTATION_CONTEXT(3)
GLOBAL_UNCERTAINTY_ASSIGNED_CONTEXT((#9969))
GLOBAL_UNIT_ASSIGNED_CONTEXT((#10021,#10023,#10024))
REPRESENTATION_CONTEXT('','3D')
);
#10003=(
GEOMETRIC_REPRESENTATION_CONTEXT(3)
GLOBAL_UNCERTAINTY_ASSIGNED_CONTEXT((#9970))
GLOBAL_UNIT_ASSIGNED_CONTEXT((#10021,#10023,#10024))
REPRESENTATION_CONTEXT('','3D')
);
#10004=(
GEOMETRIC_REPRESENTATION_CONTEXT(3)
GLOBAL_UNCERTAINTY_ASSIGNED_CONTEXT((#9971))
GLOBAL_UNIT_ASSIGNED_CONTEXT((#10021,#10023,#10024))
REPRESENTATION_CONTEXT('','3D')
);
#10005=(
GEOMETRIC_REPRESENTATION_CONTEXT(3)
GLOBAL_UNCERTAINTY_ASSIGNED_CONTEXT((#9972))
GLOBAL_UNIT_ASSIGNED_CONTEXT((#10021,#10023,#10024))
REPRESENTATION_CONTEXT('','3D')
);
#10006=(
GEOMETRIC_REPRESENTATION_CONTEXT(3)
GLOBAL_UNCERTAINTY_ASSIGNED_CONTEXT((#9973))
GLOBAL_UNIT_ASSIGNED_CONTEXT((#10021,#10023,#10024))
REPRESENTATION_CONTEXT('','3D')
);
#10007=(
GEOMETRIC_REPRESENTATION_CONTEXT(3)
GLOBAL_UNCERTAINTY_ASSIGNED_CONTEXT((#9974))
GLOBAL_UNIT_ASSIGNED_CONTEXT((#10021,#10023,#10024))
REPRESENTATION_CONTEXT('','3D')
);
#10008=(
GEOMETRIC_REPRESENTATION_CONTEXT(3)
GLOBAL_UNCERTAINTY_ASSIGNED_CONTEXT((#9975))
GLOBAL_UNIT_ASSIGNED_CONTEXT((#10021,#10023,#10024))
REPRESENTATION_CONTEXT('','3D')
);
#10009=(
GEOMETRIC_REPRESENTATION_CONTEXT(3)
GLOBAL_UNCERTAINTY_ASSIGNED_CONTEXT((#9976))
GLOBAL_UNIT_ASSIGNED_CONTEXT((#10021,#10023,#10024))
REPRESENTATION_CONTEXT('','3D')
);
#10010=(
GEOMETRIC_REPRESENTATION_CONTEXT(3)
GLOBAL_UNCERTAINTY_ASSIGNED_CONTEXT((#9977))
GLOBAL_UNIT_ASSIGNED_CONTEXT((#10021,#10023,#10024))
REPRESENTATION_CONTEXT('','3D')
);
#10011=(
GEOMETRIC_REPRESENTATION_CONTEXT(3)
GLOBAL_UNCERTAINTY_ASSIGNED_CONTEXT((#9978))
GLOBAL_UNIT_ASSIGNED_CONTEXT((#10021,#10023,#10024))
REPRESENTATION_CONTEXT('','3D')
);
#10012=(
GEOMETRIC_REPRESENTATION_CONTEXT(3)
GLOBAL_UNCERTAINTY_ASSIGNED_CONTEXT((#9979))
GLOBAL_UNIT_ASSIGNED_CONTEXT((#10021,#10023,#10024))
REPRESENTATION_CONTEXT('','3D')
);
#10013=(
GEOMETRIC_REPRESENTATION_CONTEXT(3)
GLOBAL_UNCERTAINTY_ASSIGNED_CONTEXT((#9980))
GLOBAL_UNIT_ASSIGNED_CONTEXT((#10021,#10023,#10024))
REPRESENTATION_CONTEXT('','3D')
);
#10014=(
GEOMETRIC_REPRESENTATION_CONTEXT(3)
GLOBAL_UNCERTAINTY_ASSIGNED_CONTEXT((#9981))
GLOBAL_UNIT_ASSIGNED_CONTEXT((#10021,#10023,#10024))
REPRESENTATION_CONTEXT('','3D')
);
#10015=(
GEOMETRIC_REPRESENTATION_CONTEXT(3)
GLOBAL_UNCERTAINTY_ASSIGNED_CONTEXT((#9982))
GLOBAL_UNIT_ASSIGNED_CONTEXT((#10021,#10023,#10024))
REPRESENTATION_CONTEXT('','3D')
);
#10016=(
GEOMETRIC_REPRESENTATION_CONTEXT(3)
GLOBAL_UNCERTAINTY_ASSIGNED_CONTEXT((#9983))
GLOBAL_UNIT_ASSIGNED_CONTEXT((#10021,#10023,#10024))
REPRESENTATION_CONTEXT('','3D')
);
#10017=(
GEOMETRIC_REPRESENTATION_CONTEXT(3)
GLOBAL_UNCERTAINTY_ASSIGNED_CONTEXT((#9984))
GLOBAL_UNIT_ASSIGNED_CONTEXT((#10021,#10023,#10024))
REPRESENTATION_CONTEXT('','3D')
);
#10018=(
GEOMETRIC_REPRESENTATION_CONTEXT(3)
GLOBAL_UNCERTAINTY_ASSIGNED_CONTEXT((#9985))
GLOBAL_UNIT_ASSIGNED_CONTEXT((#10021,#10023,#10024))
REPRESENTATION_CONTEXT('','3D')
);
#10019=(
GEOMETRIC_REPRESENTATION_CONTEXT(3)
GLOBAL_UNCERTAINTY_ASSIGNED_CONTEXT((#9986))
GLOBAL_UNIT_ASSIGNED_CONTEXT((#10021,#10023,#10024))
REPRESENTATION_CONTEXT('','3D')
);
#10020=(
GEOMETRIC_REPRESENTATION_CONTEXT(3)
GLOBAL_UNCERTAINTY_ASSIGNED_CONTEXT((#9987))
GLOBAL_UNIT_ASSIGNED_CONTEXT((#10021,#10023,#10024))
REPRESENTATION_CONTEXT('','3D')
);
#10021=(
LENGTH_UNIT()
NAMED_UNIT(*)
SI_UNIT(.CENTI.,.METRE.)
);
#10022=(
LENGTH_UNIT()
NAMED_UNIT(*)
SI_UNIT($,.METRE.)
);
#10023=(
NAMED_UNIT(*)
PLANE_ANGLE_UNIT()
SI_UNIT($,.RADIAN.)
);
#10024=(
NAMED_UNIT(*)
SI_UNIT($,.STERADIAN.)
SOLID_ANGLE_UNIT()
);
#10025=SHAPE_DEFINITION_REPRESENTATION(#10057,#10135);
#10026=SHAPE_DEFINITION_REPRESENTATION(#10058,#10136);
#10027=SHAPE_DEFINITION_REPRESENTATION(#10059,#10137);
#10028=SHAPE_DEFINITION_REPRESENTATION(#10060,#10138);
#10029=SHAPE_DEFINITION_REPRESENTATION(#10061,#10139);
#10030=SHAPE_DEFINITION_REPRESENTATION(#10062,#10140);
#10031=SHAPE_DEFINITION_REPRESENTATION(#10063,#10141);
#10032=SHAPE_DEFINITION_REPRESENTATION(#10064,#10142);
#10033=SHAPE_DEFINITION_REPRESENTATION(#10065,#10143);
#10034=SHAPE_DEFINITION_REPRESENTATION(#10066,#10144);
#10035=SHAPE_DEFINITION_REPRESENTATION(#10067,#10145);
#10036=SHAPE_DEFINITION_REPRESENTATION(#10068,#10146);
#10037=SHAPE_DEFINITION_REPRESENTATION(#10069,#10147);
#10038=SHAPE_DEFINITION_REPRESENTATION(#10070,#10148);
#10039=SHAPE_DEFINITION_REPRESENTATION(#10071,#10149);
#10040=SHAPE_DEFINITION_REPRESENTATION(#10072,#10150);
#10041=SHAPE_DEFINITION_REPRESENTATION(#10073,#10151);
#10042=SHAPE_DEFINITION_REPRESENTATION(#10074,#10152);
#10043=SHAPE_DEFINITION_REPRESENTATION(#10075,#10153);
#10044=SHAPE_DEFINITION_REPRESENTATION(#10076,#10154);
#10045=SHAPE_DEFINITION_REPRESENTATION(#10077,#10155);
#10046=SHAPE_DEFINITION_REPRESENTATION(#10083,#10156);
#10047=SHAPE_DEFINITION_REPRESENTATION(#10084,#10157);
#10048=SHAPE_DEFINITION_REPRESENTATION(#10085,#10158);
#10049=SHAPE_DEFINITION_REPRESENTATION(#10086,#10159);
#10050=SHAPE_DEFINITION_REPRESENTATION(#10087,#10160);
#10051=SHAPE_DEFINITION_REPRESENTATION(#10088,#10161);
#10052=SHAPE_DEFINITION_REPRESENTATION(#10089,#10162);
#10053=SHAPE_DEFINITION_REPRESENTATION(#10125,#10163);
#10054=SHAPE_DEFINITION_REPRESENTATION(#10126,#10164);
#10055=SHAPE_DEFINITION_REPRESENTATION(#10127,#10165);
#10056=SHAPE_DEFINITION_REPRESENTATION(#10128,#10166);
#10057=PRODUCT_DEFINITION_SHAPE('',$,#10168);
#10058=PRODUCT_DEFINITION_SHAPE('',$,#10169);
#10059=PRODUCT_DEFINITION_SHAPE('',$,#10170);
#10060=PRODUCT_DEFINITION_SHAPE('',$,#10171);
#10061=PRODUCT_DEFINITION_SHAPE('',$,#10172);
#10062=PRODUCT_DEFINITION_SHAPE('',$,#10173);
#10063=PRODUCT_DEFINITION_SHAPE('',$,#10174);
#10064=PRODUCT_DEFINITION_SHAPE('',$,#10175);
#10065=PRODUCT_DEFINITION_SHAPE('',$,#10176);
#10066=PRODUCT_DEFINITION_SHAPE('',$,#10177);
#10067=PRODUCT_DEFINITION_SHAPE('',$,#10178);
#10068=PRODUCT_DEFINITION_SHAPE('',$,#10179);
#10069=PRODUCT_DEFINITION_SHAPE('',$,#10180);
#10070=PRODUCT_DEFINITION_SHAPE('',$,#10181);
#10071=PRODUCT_DEFINITION_SHAPE('',$,#10182);
#10072=PRODUCT_DEFINITION_SHAPE('',$,#10183);
#10073=PRODUCT_DEFINITION_SHAPE('',$,#10184);
#10074=PRODUCT_DEFINITION_SHAPE('',$,#10185);
#10075=PRODUCT_DEFINITION_SHAPE('',$,#10186);
#10076=PRODUCT_DEFINITION_SHAPE('',$,#10187);
#10077=PRODUCT_DEFINITION_SHAPE('',$,#10188);
#10078=PRODUCT_DEFINITION_SHAPE($,$,#149);
#10079=PRODUCT_DEFINITION_SHAPE($,$,#150);
#10080=PRODUCT_DEFINITION_SHAPE($,$,#151);
#10081=PRODUCT_DEFINITION_SHAPE($,$,#152);
#10082=PRODUCT_DEFINITION_SHAPE($,$,#153);
#10083=PRODUCT_DEFINITION_SHAPE('',$,#10189);
#10084=PRODUCT_DEFINITION_SHAPE('',$,#10190);
#10085=PRODUCT_DEFINITION_SHAPE('',$,#10191);
#10086=PRODUCT_DEFINITION_SHAPE('',$,#10192);
#10087=PRODUCT_DEFINITION_SHAPE('',$,#10193);
#10088=PRODUCT_DEFINITION_SHAPE('',$,#10194);
#10089=PRODUCT_DEFINITION_SHAPE('',$,#10195);
#10090=PRODUCT_DEFINITION_SHAPE($,$,#154);
#10091=PRODUCT_DEFINITION_SHAPE($,$,#155);
#10092=PRODUCT_DEFINITION_SHAPE($,$,#156);
#10093=PRODUCT_DEFINITION_SHAPE($,$,#157);
#10094=PRODUCT_DEFINITION_SHAPE($,$,#158);
#10095=PRODUCT_DEFINITION_SHAPE($,$,#159);
#10096=PRODUCT_DEFINITION_SHAPE($,$,#160);
#10097=PRODUCT_DEFINITION_SHAPE($,$,#161);
#10098=PRODUCT_DEFINITION_SHAPE($,$,#162);
#10099=PRODUCT_DEFINITION_SHAPE($,$,#163);
#10100=PRODUCT_DEFINITION_SHAPE($,$,#164);
#10101=PRODUCT_DEFINITION_SHAPE($,$,#165);
#10102=PRODUCT_DEFINITION_SHAPE($,$,#166);
#10103=PRODUCT_DEFINITION_SHAPE($,$,#167);
#10104=PRODUCT_DEFINITION_SHAPE($,$,#168);
#10105=PRODUCT_DEFINITION_SHAPE($,$,#169);
#10106=PRODUCT_DEFINITION_SHAPE($,$,#170);
#10107=PRODUCT_DEFINITION_SHAPE($,$,#171);
#10108=PRODUCT_DEFINITION_SHAPE($,$,#172);
#10109=PRODUCT_DEFINITION_SHAPE($,$,#173);
#10110=PRODUCT_DEFINITION_SHAPE($,$,#174);
#10111=PRODUCT_DEFINITION_SHAPE($,$,#175);
#10112=PRODUCT_DEFINITION_SHAPE($,$,#176);
#10113=PRODUCT_DEFINITION_SHAPE($,$,#177);
#10114=PRODUCT_DEFINITION_SHAPE($,$,#178);
#10115=PRODUCT_DEFINITION_SHAPE($,$,#179);
#10116=PRODUCT_DEFINITION_SHAPE($,$,#180);
#10117=PRODUCT_DEFINITION_SHAPE($,$,#181);
#10118=PRODUCT_DEFINITION_SHAPE($,$,#182);
#10119=PRODUCT_DEFINITION_SHAPE($,$,#183);
#10120=PRODUCT_DEFINITION_SHAPE($,$,#184);
#10121=PRODUCT_DEFINITION_SHAPE($,$,#185);
#10122=PRODUCT_DEFINITION_SHAPE($,$,#186);
#10123=PRODUCT_DEFINITION_SHAPE($,$,#187);
#10124=PRODUCT_DEFINITION_SHAPE($,$,#188);
#10125=PRODUCT_DEFINITION_SHAPE('',$,#10196);
#10126=PRODUCT_DEFINITION_SHAPE('',$,#10197);
#10127=PRODUCT_DEFINITION_SHAPE('',$,#10198);
#10128=PRODUCT_DEFINITION_SHAPE('',$,#10199);
#10129=PRODUCT_DEFINITION_SHAPE($,$,#189);
#10130=PRODUCT_DEFINITION_SHAPE($,$,#190);
#10131=PRODUCT_DEFINITION_SHAPE($,$,#191);
#10132=PRODUCT_DEFINITION_SHAPE($,$,#192);
#10133=PRODUCT_DEFINITION_SHAPE($,$,#193);
#10134=PRODUCT_DEFINITION_SHAPE($,$,#194);
#10135=SHAPE_REPRESENTATION('',(#4907,#5570,#5571,#5572),#9988);
#10136=SHAPE_REPRESENTATION('',(#4908,#5486,#5487,#5488,#5489,#5490,#5491,
#5492,#5493,#5494,#5495,#5496,#5497,#5498,#5499,#5500,#5501,#5502,#5503,
#5504,#5505,#5506,#5507,#5508),#9989);
#10137=SHAPE_REPRESENTATION('',(#4909),#9990);
#10138=SHAPE_REPRESENTATION('',(#4937),#9991);
#10139=SHAPE_REPRESENTATION('',(#4943),#9992);
#10140=SHAPE_REPRESENTATION('',(#4949),#9993);
#10141=SHAPE_REPRESENTATION('',(#4955),#9994);
#10142=SHAPE_REPRESENTATION('',(#4961),#9995);
#10143=SHAPE_REPRESENTATION('',(#4991),#9996);
#10144=SHAPE_REPRESENTATION('',(#5000),#9997);
#10145=SHAPE_REPRESENTATION('',(#5014),#9998);
#10146=SHAPE_REPRESENTATION('',(#5033),#9999);
#10147=SHAPE_REPRESENTATION('',(#5046),#10000);
#10148=SHAPE_REPRESENTATION('',(#5051),#10001);
#10149=SHAPE_REPRESENTATION('',(#5060),#10002);
#10150=SHAPE_REPRESENTATION('',(#5084,#5223,#5224,#5225,#5226,#5227),#10003);
#10151=SHAPE_REPRESENTATION('',(#5085),#10004);
#10152=SHAPE_REPRESENTATION('',(#5105),#10005);
#10153=SHAPE_REPRESENTATION('',(#5125),#10006);
#10154=SHAPE_REPRESENTATION('',(#5144),#10007);
#10155=SHAPE_REPRESENTATION('',(#5206),#10008);
#10156=SHAPE_REPRESENTATION('',(#5228),#10009);
#10157=SHAPE_REPRESENTATION('',(#5243,#5509,#5510,#5511,#5512,#5513,#5514,
#5515,#5516,#5517,#5518,#5519,#5520),#10010);
#10158=SHAPE_REPRESENTATION('',(#5244),#10011);
#10159=SHAPE_REPRESENTATION('',(#5369),#10012);
#10160=SHAPE_REPRESENTATION('',(#5378),#10013);
#10161=SHAPE_REPRESENTATION('',(#5403),#10014);
#10162=SHAPE_REPRESENTATION('',(#5460),#10015);
#10163=SHAPE_REPRESENTATION('',(#5521,#5567,#5568,#5569),#10016);
#10164=SHAPE_REPRESENTATION('',(#5522),#10017);
#10165=SHAPE_REPRESENTATION('',(#5536),#10018);
#10166=SHAPE_REPRESENTATION('',(#5550),#10019);
#10167=PRODUCT_DEFINITION_CONTEXT('part definition',#10265,'design');
#10168=PRODUCT_DEFINITION('PAT-060',
'PAT-060',#10200,#10167);
#10169=PRODUCT_DEFINITION('Base and spindle','Base and spindle',#10201,
#10167);
#10170=PRODUCT_DEFINITION('Base','Base',#10202,#10167);
#10171=PRODUCT_DEFINITION('Bonded foot','Bonded foot',#10203,#10167);
#10172=PRODUCT_DEFINITION('Bonded foot (1)','Bonded foot (1)',#10204,#10167);
#10173=PRODUCT_DEFINITION('Bonded foot (2)','Bonded foot (2)',#10205,#10167);
#10174=PRODUCT_DEFINITION('Bonded foot (3)','Bonded foot (3)',#10206,#10167);
#10175=PRODUCT_DEFINITION('Fixed spindle','Fixed spindle',#10207,#10167);
#10176=PRODUCT_DEFINITION('Inner race spacer','Inner race spacer',#10208,
#10167);
#10177=PRODUCT_DEFINITION('Spindle collar','Spindle collar',#10209,#10167);
#10178=PRODUCT_DEFINITION('Plunger mounting gland',
'Plunger mounting gland',#10210,#10167);
#10179=PRODUCT_DEFINITION('Plunger body','Plunger body',#10211,#10167);
#10180=PRODUCT_DEFINITION('Installed compression spring',
'Installed compression spring',#10212,#10167);
#10181=PRODUCT_DEFINITION('Flat Washer - M6','Flat Washer - M6',#10213,
#10167);
#10182=PRODUCT_DEFINITION('M6x18 mounting screw','M6x18 mounting screw',
#10214,#10167);
#10183=PRODUCT_DEFINITION('Sealed Ball Bearing - 25 x 52 x 15 mm',
'Sealed Ball Bearing - 25 x 52 x 15 mm',#10215,#10167);
#10184=PRODUCT_DEFINITION('Inner ring','Inner ring',#10216,#10167);
#10185=PRODUCT_DEFINITION('Outer ring','Outer ring',#10217,#10167);
#10186=PRODUCT_DEFINITION('Balls','Balls',#10218,#10167);
#10187=PRODUCT_DEFINITION('Cage','Cage',#10219,#10167);
#10188=PRODUCT_DEFINITION('Seals 2RS','Seals 2RS',#10220,#10167);
#10189=PRODUCT_DEFINITION('M5x5 collar screw','M5x5 collar screw',#10221,
#10167);
#10190=PRODUCT_DEFINITION('Indexed table','Indexed table',#10222,#10167);
#10191=PRODUCT_DEFINITION('Index table','Index table',#10223,#10167);
#10192=PRODUCT_DEFINITION('Outer race spacer','Outer race spacer',#10224,
#10167);
#10193=PRODUCT_DEFINITION('Lower bearing cap','Lower bearing cap',#10225,
#10167);
#10194=PRODUCT_DEFINITION('Detent ring','Detent ring',#10226,#10167);
#10195=PRODUCT_DEFINITION('Cap Screw - M4x16','Cap Screw - M4x16',#10227,
#10167);
#10196=PRODUCT_DEFINITION('Release plunger','Release plunger',#10228,#10167);
#10197=PRODUCT_DEFINITION('Detent pin','Detent pin',#10229,#10167);
#10198=PRODUCT_DEFINITION('Release knob','Release knob',#10230,#10167);
#10199=PRODUCT_DEFINITION('Socket Set Screw - M5x8',
'Socket Set Screw - M5x8',#10231,#10167);
#10200=PRODUCT_DEFINITION_FORMATION('',$,#10267);
#10201=PRODUCT_DEFINITION_FORMATION('',$,#10268);
#10202=PRODUCT_DEFINITION_FORMATION('',$,#10269);
#10203=PRODUCT_DEFINITION_FORMATION('',$,#10270);
#10204=PRODUCT_DEFINITION_FORMATION('',$,#10271);
#10205=PRODUCT_DEFINITION_FORMATION('',$,#10272);
#10206=PRODUCT_DEFINITION_FORMATION('',$,#10273);
#10207=PRODUCT_DEFINITION_FORMATION('',$,#10274);
#10208=PRODUCT_DEFINITION_FORMATION('',$,#10275);
#10209=PRODUCT_DEFINITION_FORMATION('',$,#10276);
#10210=PRODUCT_DEFINITION_FORMATION('',$,#10277);
#10211=PRODUCT_DEFINITION_FORMATION('',$,#10278);
#10212=PRODUCT_DEFINITION_FORMATION('',$,#10279);
#10213=PRODUCT_DEFINITION_FORMATION('',$,#10280);
#10214=PRODUCT_DEFINITION_FORMATION('',$,#10281);
#10215=PRODUCT_DEFINITION_FORMATION('',$,#10282);
#10216=PRODUCT_DEFINITION_FORMATION('',$,#10283);
#10217=PRODUCT_DEFINITION_FORMATION('',$,#10284);
#10218=PRODUCT_DEFINITION_FORMATION('',$,#10285);
#10219=PRODUCT_DEFINITION_FORMATION('',$,#10286);
#10220=PRODUCT_DEFINITION_FORMATION('',$,#10287);
#10221=PRODUCT_DEFINITION_FORMATION('',$,#10288);
#10222=PRODUCT_DEFINITION_FORMATION('',$,#10289);
#10223=PRODUCT_DEFINITION_FORMATION('',$,#10290);
#10224=PRODUCT_DEFINITION_FORMATION('',$,#10291);
#10225=PRODUCT_DEFINITION_FORMATION('',$,#10292);
#10226=PRODUCT_DEFINITION_FORMATION('',$,#10293);
#10227=PRODUCT_DEFINITION_FORMATION('',$,#10294);
#10228=PRODUCT_DEFINITION_FORMATION('',$,#10295);
#10229=PRODUCT_DEFINITION_FORMATION('',$,#10296);
#10230=PRODUCT_DEFINITION_FORMATION('',$,#10297);
#10231=PRODUCT_DEFINITION_FORMATION('',$,#10298);
#10232=PRODUCT_RELATED_PRODUCT_CATEGORY('PAT-060','PAT-060',(#10267));
#10233=PRODUCT_RELATED_PRODUCT_CATEGORY('Base and spindle',
'Base and spindle',(#10268));
#10234=PRODUCT_RELATED_PRODUCT_CATEGORY('Base','Base',(#10269));
#10235=PRODUCT_RELATED_PRODUCT_CATEGORY('Bonded foot','Bonded foot',(#10270));
#10236=PRODUCT_RELATED_PRODUCT_CATEGORY('Bonded foot (1)',
'Bonded foot (1)',(#10271));
#10237=PRODUCT_RELATED_PRODUCT_CATEGORY('Bonded foot (2)',
'Bonded foot (2)',(#10272));
#10238=PRODUCT_RELATED_PRODUCT_CATEGORY('Bonded foot (3)',
'Bonded foot (3)',(#10273));
#10239=PRODUCT_RELATED_PRODUCT_CATEGORY('Fixed spindle','Fixed spindle',
(#10274));
#10240=PRODUCT_RELATED_PRODUCT_CATEGORY('Inner race spacer',
'Inner race spacer',(#10275));
#10241=PRODUCT_RELATED_PRODUCT_CATEGORY('Spindle collar',
'Spindle collar',(#10276));
#10242=PRODUCT_RELATED_PRODUCT_CATEGORY('Plunger mounting gland',
'Plunger mounting gland',(#10277));
#10243=PRODUCT_RELATED_PRODUCT_CATEGORY('Plunger body','Plunger body',(#10278));
#10244=PRODUCT_RELATED_PRODUCT_CATEGORY('Installed compression spring',
'Installed compression spring',(#10279));
#10245=PRODUCT_RELATED_PRODUCT_CATEGORY('Flat Washer - M6',
'Flat Washer - M6',(#10280));
#10246=PRODUCT_RELATED_PRODUCT_CATEGORY('M6x18 mounting screw',
'M6x18 mounting screw',(#10281));
#10247=PRODUCT_RELATED_PRODUCT_CATEGORY(
'Sealed Ball Bearing - 25 x 52 x 15 mm',
'Sealed Ball Bearing - 25 x 52 x 15 mm',(#10282));
#10248=PRODUCT_RELATED_PRODUCT_CATEGORY('Inner ring','Inner ring',(#10283));
#10249=PRODUCT_RELATED_PRODUCT_CATEGORY('Outer ring','Outer ring',(#10284));
#10250=PRODUCT_RELATED_PRODUCT_CATEGORY('Balls','Balls',(#10285));
#10251=PRODUCT_RELATED_PRODUCT_CATEGORY('Cage','Cage',(#10286));
#10252=PRODUCT_RELATED_PRODUCT_CATEGORY('Seals 2RS','Seals 2RS',(#10287));
#10253=PRODUCT_RELATED_PRODUCT_CATEGORY('M5x5 collar screw',
'M5x5 collar screw',(#10288));
#10254=PRODUCT_RELATED_PRODUCT_CATEGORY('Indexed table','Indexed table',
(#10289));
#10255=PRODUCT_RELATED_PRODUCT_CATEGORY('Index table','Index table',(#10290));
#10256=PRODUCT_RELATED_PRODUCT_CATEGORY('Outer race spacer',
'Outer race spacer',(#10291));
#10257=PRODUCT_RELATED_PRODUCT_CATEGORY('Lower bearing cap',
'Lower bearing cap',(#10292));
#10258=PRODUCT_RELATED_PRODUCT_CATEGORY('Detent ring','Detent ring',(#10293));
#10259=PRODUCT_RELATED_PRODUCT_CATEGORY('Cap Screw - M4x16',
'Cap Screw - M4x16',(#10294));
#10260=PRODUCT_RELATED_PRODUCT_CATEGORY('Release plunger',
'Release plunger',(#10295));
#10261=PRODUCT_RELATED_PRODUCT_CATEGORY('Detent pin','Detent pin',(#10296));
#10262=PRODUCT_RELATED_PRODUCT_CATEGORY('Release knob','Release knob',(#10297));
#10263=PRODUCT_RELATED_PRODUCT_CATEGORY('Socket Set Screw - M5x8',
'Socket Set Screw - M5x8',(#10298));
#10264=APPLICATION_PROTOCOL_DEFINITION('international standard',
'automotive_design',2009,#10265);
#10265=APPLICATION_CONTEXT(
'Core Data for Automotive Mechanical Design Process');
#10266=PRODUCT_CONTEXT('part definition',#10265,'mechanical');
#10267=PRODUCT('PAT-060','PAT-060',
'PAT-060',(#10266));
#10268=PRODUCT('Base and spindle','Base and spindle','Base and spindle',
(#10266));
#10269=PRODUCT('Base','Base','Base',(#10266));
#10270=PRODUCT('Bonded foot','Bonded foot','Bonded foot',(#10266));
#10271=PRODUCT('Bonded foot (1)','Bonded foot (1)','Bonded foot (1)',(#10266));
#10272=PRODUCT('Bonded foot (2)','Bonded foot (2)','Bonded foot (2)',(#10266));
#10273=PRODUCT('Bonded foot (3)','Bonded foot (3)','Bonded foot (3)',(#10266));
#10274=PRODUCT('Fixed spindle','Fixed spindle','Fixed spindle',(#10266));
#10275=PRODUCT('Inner race spacer','Inner race spacer',
'Inner race spacer',(#10266));
#10276=PRODUCT('Spindle collar','Spindle collar','Spindle collar',(#10266));
#10277=PRODUCT('Plunger mounting gland','Plunger mounting gland',
'Plunger mounting gland',(#10266));
#10278=PRODUCT('Plunger body','Plunger body','Plunger body',(#10266));
#10279=PRODUCT('Installed compression spring',
'Installed compression spring','Installed compression spring',(#10266));
#10280=PRODUCT('Flat Washer - M6','Flat Washer - M6','Flat Washer - M6',
(#10266));
#10281=PRODUCT('M6x18 mounting screw','M6x18 mounting screw',
'M6x18 mounting screw',(#10266));
#10282=PRODUCT('Sealed Ball Bearing - 25 x 52 x 15 mm',
'Sealed Ball Bearing - 25 x 52 x 15 mm',
'Sealed Ball Bearing - 25 x 52 x 15 mm',(#10266));
#10283=PRODUCT('Inner ring','Inner ring','Inner ring',(#10266));
#10284=PRODUCT('Outer ring','Outer ring','Outer ring',(#10266));
#10285=PRODUCT('Balls','Balls','Balls',(#10266));
#10286=PRODUCT('Cage','Cage','Cage',(#10266));
#10287=PRODUCT('Seals 2RS','Seals 2RS','Seals 2RS',(#10266));
#10288=PRODUCT('M5x5 collar screw','M5x5 collar screw',
'M5x5 collar screw',(#10266));
#10289=PRODUCT('Indexed table','Indexed table','Indexed table',(#10266));
#10290=PRODUCT('Index table','Index table','Index table',(#10266));
#10291=PRODUCT('Outer race spacer','Outer race spacer',
'Outer race spacer',(#10266));
#10292=PRODUCT('Lower bearing cap','Lower bearing cap',
'Lower bearing cap',(#10266));
#10293=PRODUCT('Detent ring','Detent ring','Detent ring',(#10266));
#10294=PRODUCT('Cap Screw - M4x16','Cap Screw - M4x16',
'Cap Screw - M4x16',(#10266));
#10295=PRODUCT('Release plunger','Release plunger','Release plunger',(#10266));
#10296=PRODUCT('Detent pin','Detent pin','Detent pin',(#10266));
#10297=PRODUCT('Release knob','Release knob','Release knob',(#10266));
#10298=PRODUCT('Socket Set Screw - M5x8','Socket Set Screw - M5x8',
'Socket Set Screw - M5x8',(#10266));
#10299=PRESENTATION_STYLE_ASSIGNMENT((#10305));
#10300=PRESENTATION_STYLE_ASSIGNMENT((#10306));
#10301=PRESENTATION_STYLE_ASSIGNMENT((#10307));
#10302=PRESENTATION_STYLE_ASSIGNMENT((#10308));
#10303=PRESENTATION_STYLE_ASSIGNMENT((#10309));
#10304=PRESENTATION_STYLE_ASSIGNMENT((#10310));
#10305=SURFACE_STYLE_USAGE(.BOTH.,#10311);
#10306=SURFACE_STYLE_USAGE(.BOTH.,#10312);
#10307=SURFACE_STYLE_USAGE(.BOTH.,#10313);
#10308=SURFACE_STYLE_USAGE(.BOTH.,#10314);
#10309=SURFACE_STYLE_USAGE(.BOTH.,#10315);
#10310=SURFACE_STYLE_USAGE(.BOTH.,#10316);
#10311=SURFACE_SIDE_STYLE('',(#10317));
#10312=SURFACE_SIDE_STYLE('',(#10318));
#10313=SURFACE_SIDE_STYLE('',(#10319));
#10314=SURFACE_SIDE_STYLE('',(#10320));
#10315=SURFACE_SIDE_STYLE('',(#10321));
#10316=SURFACE_SIDE_STYLE('',(#10322));
#10317=SURFACE_STYLE_FILL_AREA(#10323);
#10318=SURFACE_STYLE_FILL_AREA(#10324);
#10319=SURFACE_STYLE_FILL_AREA(#10325);
#10320=SURFACE_STYLE_FILL_AREA(#10326);
#10321=SURFACE_STYLE_FILL_AREA(#10327);
#10322=SURFACE_STYLE_FILL_AREA(#10328);
#10323=FILL_AREA_STYLE('Steel - Satin',(#10329));
#10324=FILL_AREA_STYLE('CAD Library Painted - Deep blue',(#10330));
#10325=FILL_AREA_STYLE('CAD Library Painted - Engineering blue',(#10331));
#10326=FILL_AREA_STYLE('CAD Library Painted - Steel gray',(#10332));
#10327=FILL_AREA_STYLE('CAD Library Painted - Graphite',(#10333));
#10328=FILL_AREA_STYLE('CAD Library Painted - Light blue',(#10334));
#10329=FILL_AREA_STYLE_COLOUR('Steel - Satin',#10335);
#10330=FILL_AREA_STYLE_COLOUR('CAD Library Painted - Deep blue',#10336);
#10331=FILL_AREA_STYLE_COLOUR('CAD Library Painted - Engineering blue',
#10337);
#10332=FILL_AREA_STYLE_COLOUR('CAD Library Painted - Steel gray',#10338);
#10333=FILL_AREA_STYLE_COLOUR('CAD Library Painted - Graphite',#10339);
#10334=FILL_AREA_STYLE_COLOUR('CAD Library Painted - Light blue',#10340);
#10335=COLOUR_RGB('Steel - Satin',0.627450980392157,0.627450980392157,0.627450980392157);
#10336=COLOUR_RGB('CAD Library Painted - Deep blue',0.0784313725490196,
0.203921568627451,0.349019607843137);
#10337=COLOUR_RGB('CAD Library Painted - Engineering blue',0.12156862745098,
0.356862745098039,0.6);
#10338=COLOUR_RGB('CAD Library Painted - Steel gray',0.592156862745098,
0.631372549019608,0.67843137254902);
#10339=COLOUR_RGB('CAD Library Painted - Graphite',0.168627450980392,0.192156862745098,
0.231372549019608);
#10340=COLOUR_RGB('CAD Library Painted - Light blue',0.286274509803922,
0.552941176470588,0.780392156862745);
#10341=COLOUR_RGB('Dark Blue',0.08,0.2,0.34);
#10342=FILL_AREA_STYLE_COLOUR('',#10341);
#10343=FILL_AREA_STYLE('',(#10342));
#10344=SURFACE_STYLE_FILL_AREA(#10343);
#10345=SURFACE_SIDE_STYLE('',(#10344));
#10346=SURFACE_STYLE_USAGE(.BOTH.,#10345);
#10347=PRESENTATION_STYLE_ASSIGNMENT((#10346));
#10348=COLOUR_RGB('Light Blue',0.38,0.62,0.78);
#10349=FILL_AREA_STYLE_COLOUR('',#10348);
#10350=FILL_AREA_STYLE('',(#10349));
#10351=SURFACE_STYLE_FILL_AREA(#10350);
#10352=SURFACE_SIDE_STYLE('',(#10351));
#10353=SURFACE_STYLE_USAGE(.BOTH.,#10352);
#10354=PRESENTATION_STYLE_ASSIGNMENT((#10353));
#10355=COLOUR_RGB('Sky Blue',0.24,0.69,0.87);
#10356=FILL_AREA_STYLE_COLOUR('',#10355);
#10357=FILL_AREA_STYLE('',(#10356));
#10358=SURFACE_STYLE_FILL_AREA(#10357);
#10359=SURFACE_SIDE_STYLE('',(#10358));
#10360=SURFACE_STYLE_USAGE(.BOTH.,#10359);
#10361=PRESENTATION_STYLE_ASSIGNMENT((#10360));
#10362=COLOUR_RGB('Grey',0.48,0.52,0.57);
#10363=FILL_AREA_STYLE_COLOUR('',#10362);
#10364=FILL_AREA_STYLE('',(#10363));
#10365=SURFACE_STYLE_FILL_AREA(#10364);
#10366=SURFACE_SIDE_STYLE('',(#10365));
#10367=SURFACE_STYLE_USAGE(.BOTH.,#10366);
#10368=PRESENTATION_STYLE_ASSIGNMENT((#10367));
#10369=COLOUR_RGB('Black',0.12,0.14,0.17);
#10370=FILL_AREA_STYLE_COLOUR('',#10369);
#10371=FILL_AREA_STYLE('',(#10370));
#10372=SURFACE_STYLE_FILL_AREA(#10371);
#10373=SURFACE_SIDE_STYLE('',(#10372));
#10374=SURFACE_STYLE_USAGE(.BOTH.,#10373);
#10375=PRESENTATION_STYLE_ASSIGNMENT((#10374));
#10376=COLOUR_RGB('Off White',0.89,0.88,0.83);
#10377=FILL_AREA_STYLE_COLOUR('',#10376);
#10378=FILL_AREA_STYLE('',(#10377));
#10379=SURFACE_STYLE_FILL_AREA(#10378);
#10380=SURFACE_SIDE_STYLE('',(#10379));
#10381=SURFACE_STYLE_USAGE(.BOTH.,#10380);
#10382=PRESENTATION_STYLE_ASSIGNMENT((#10381));
ENDSEC;
END-ISO-10303-21;
